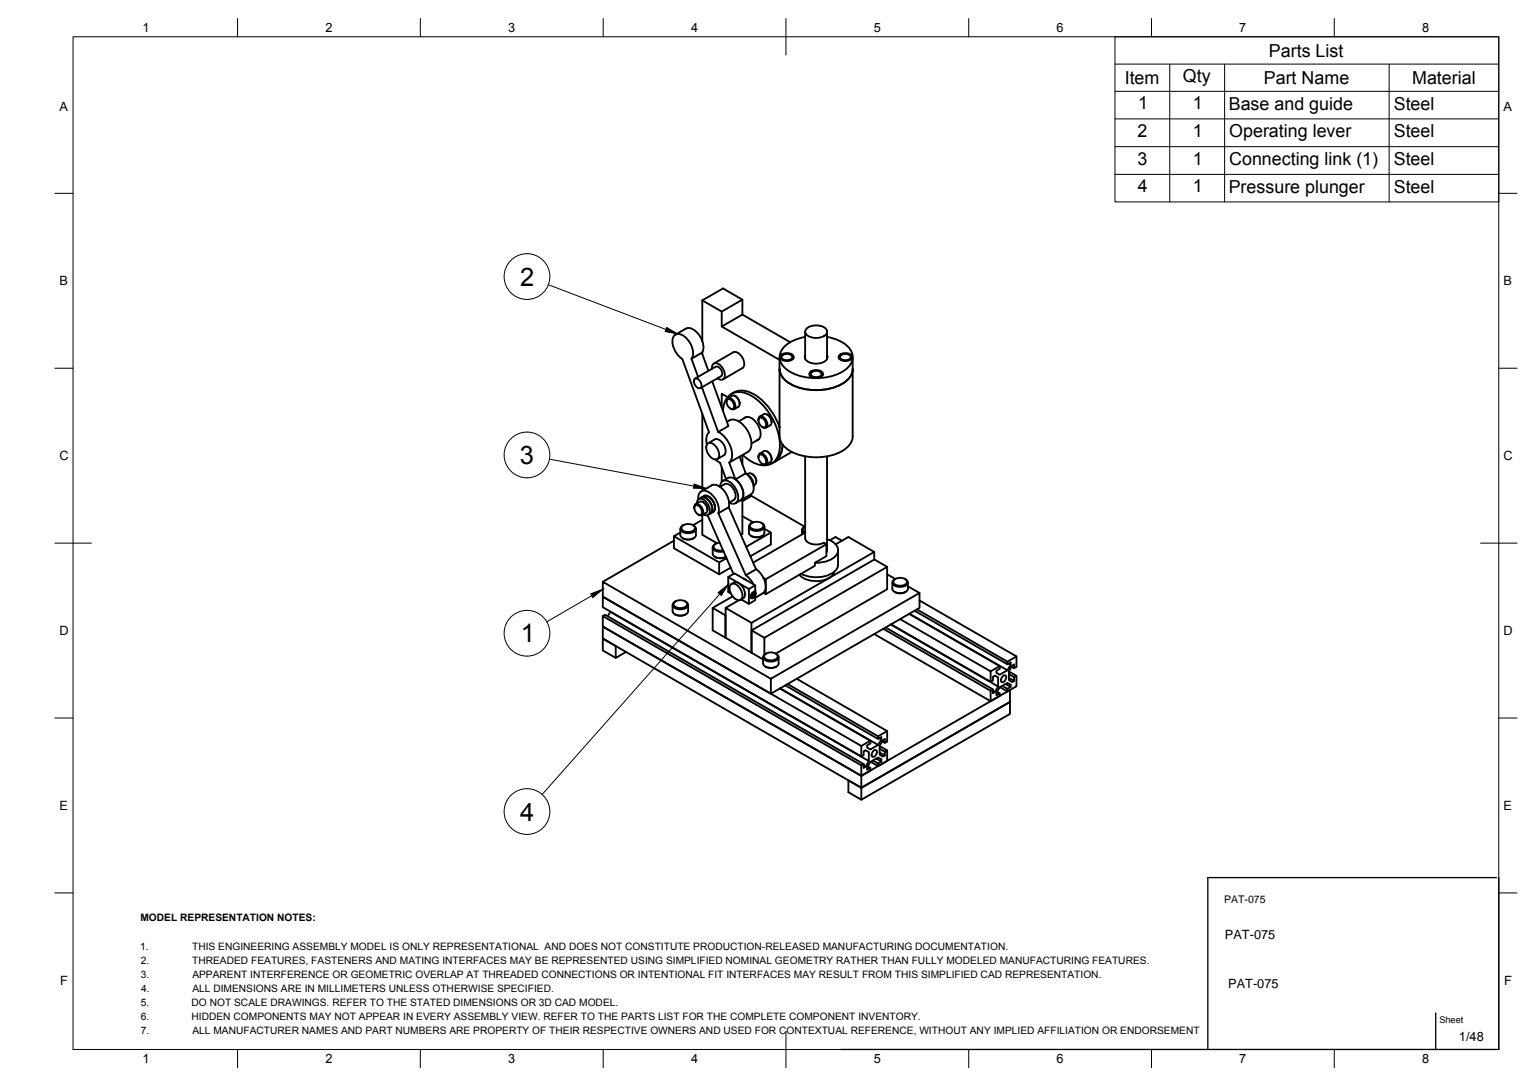
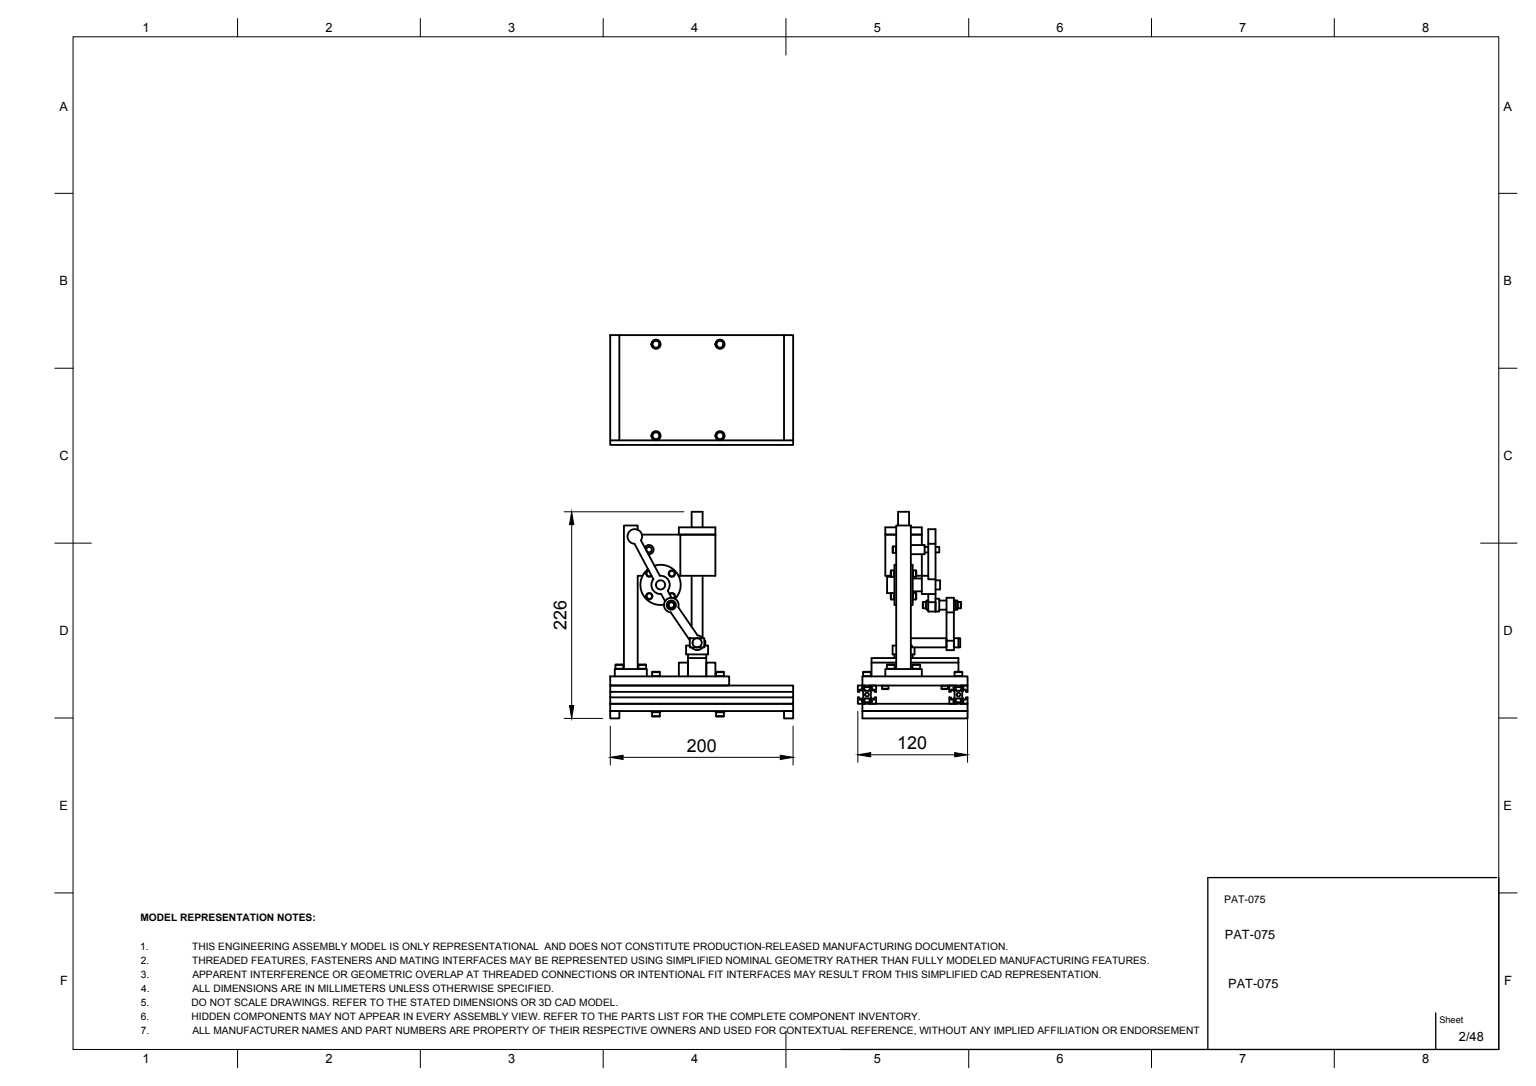
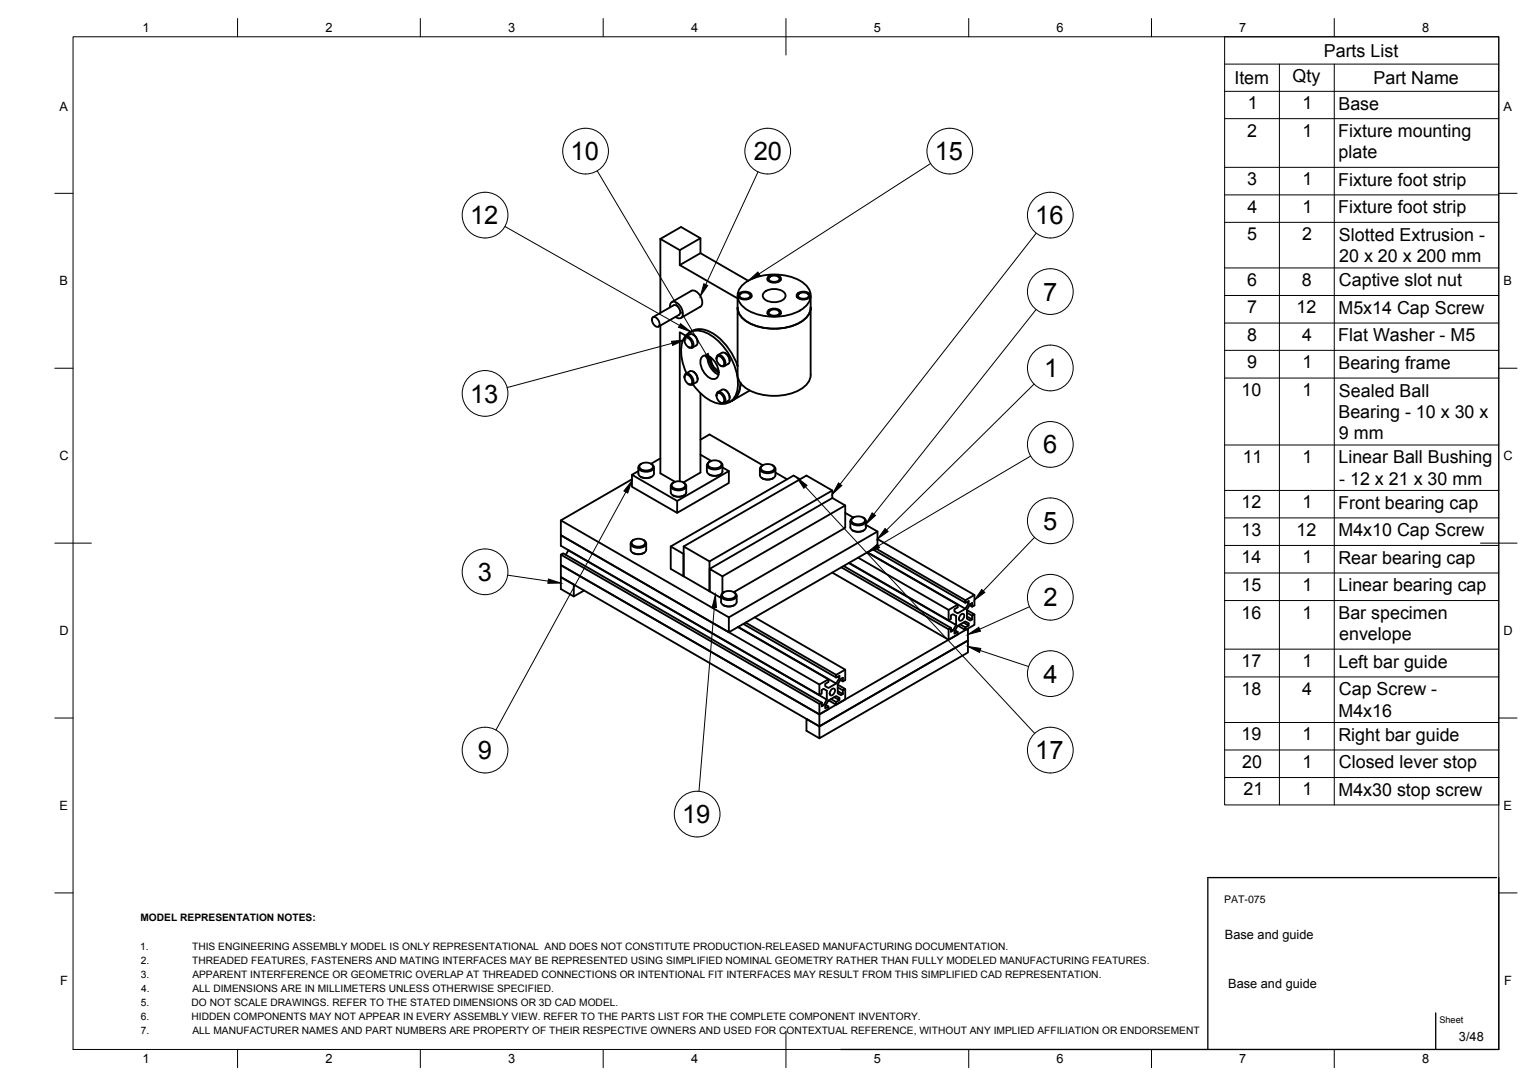
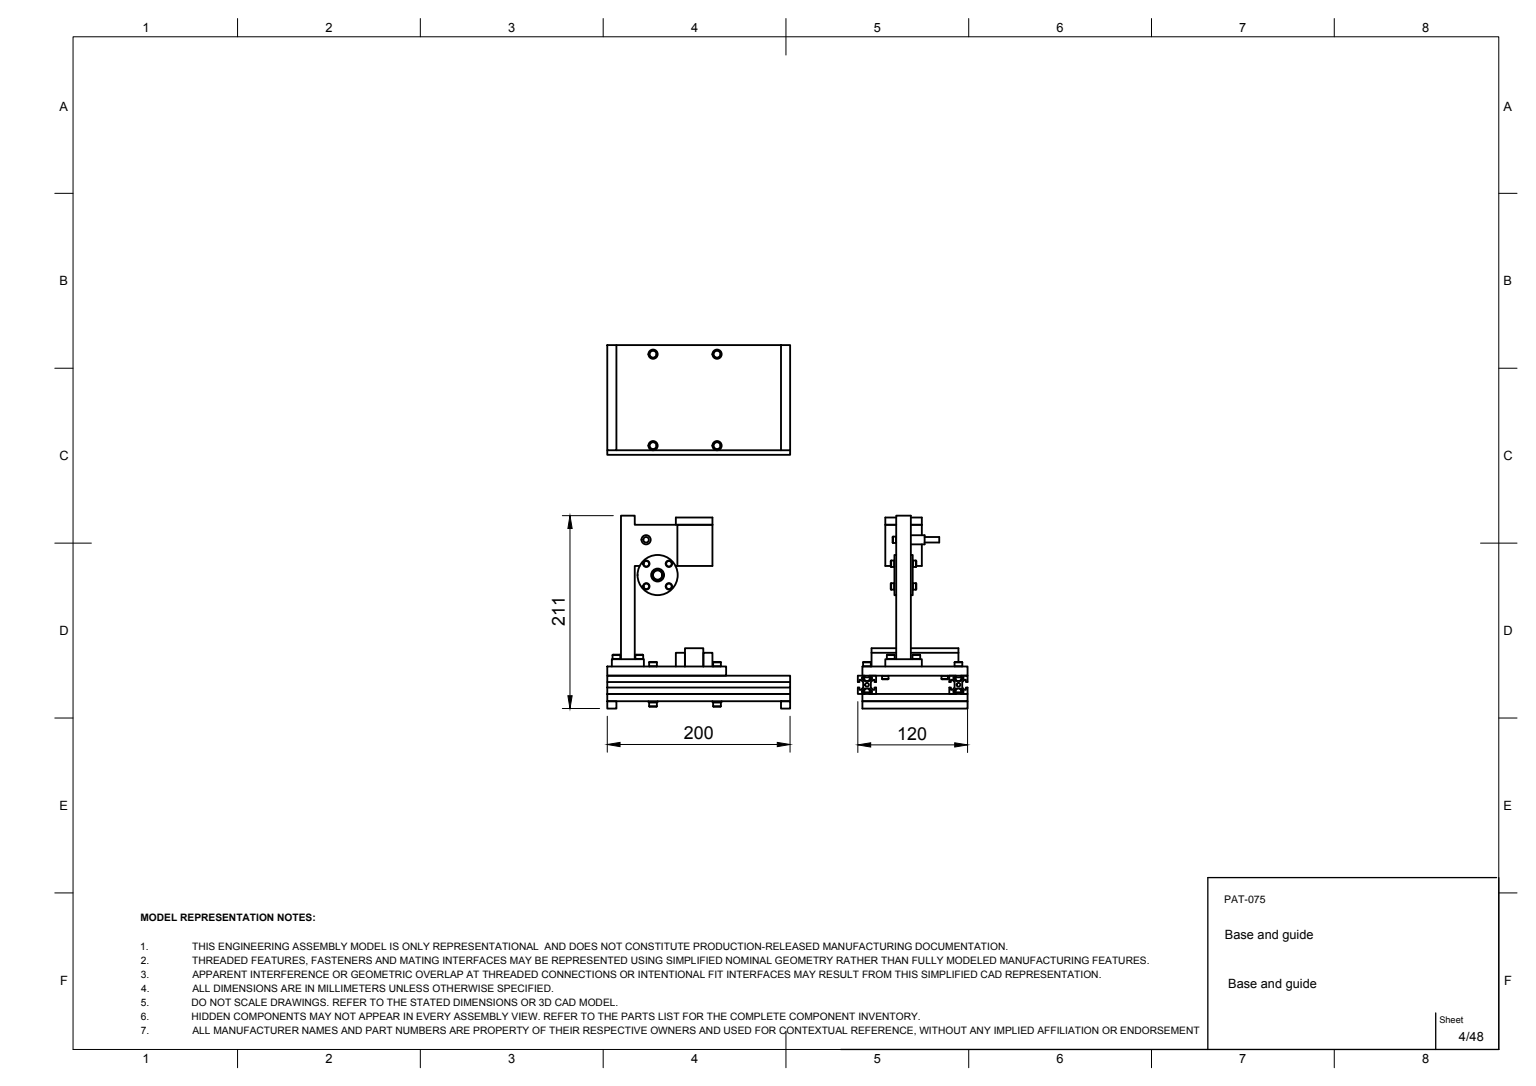
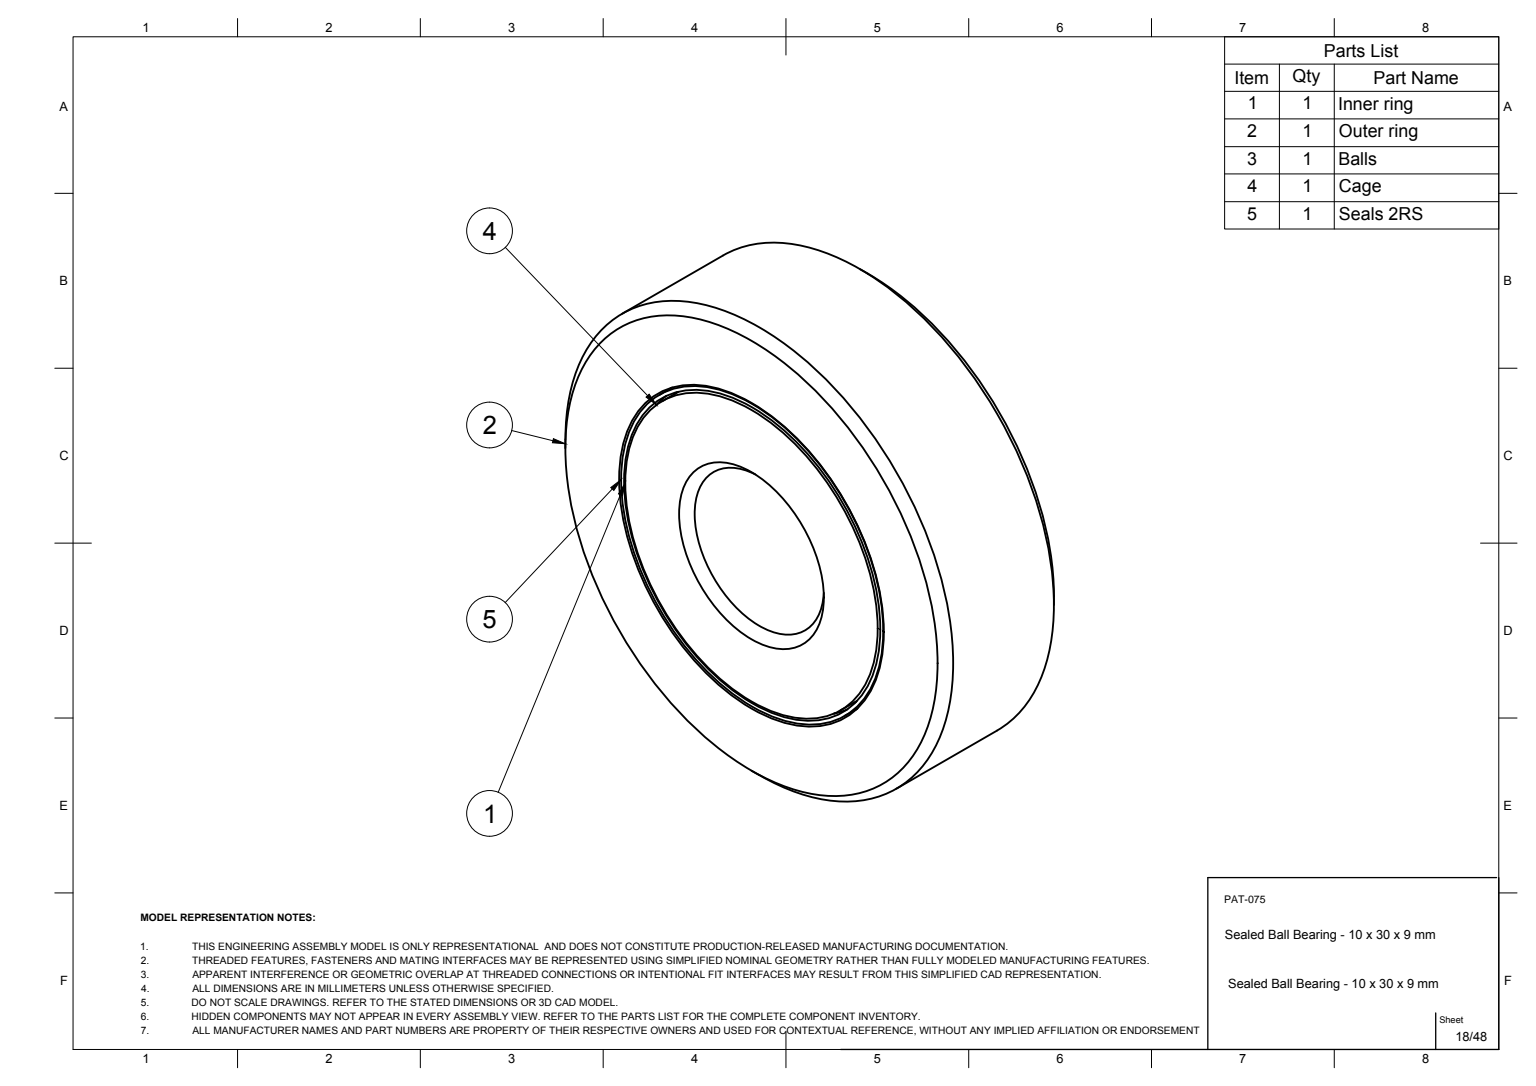
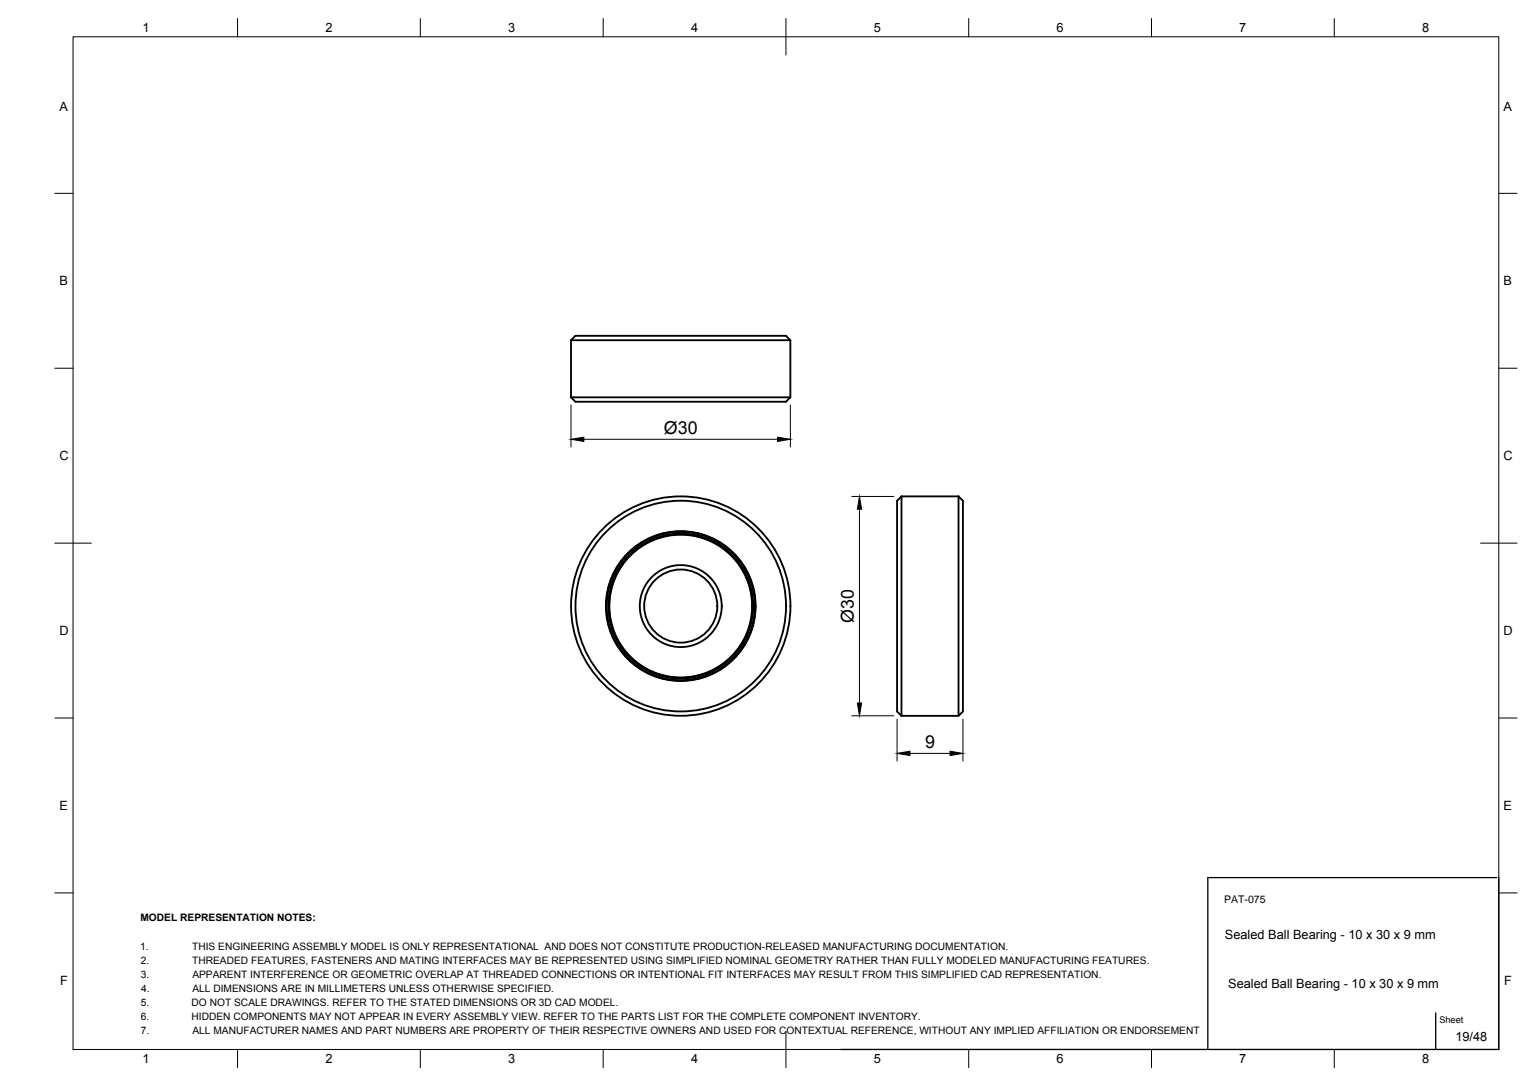
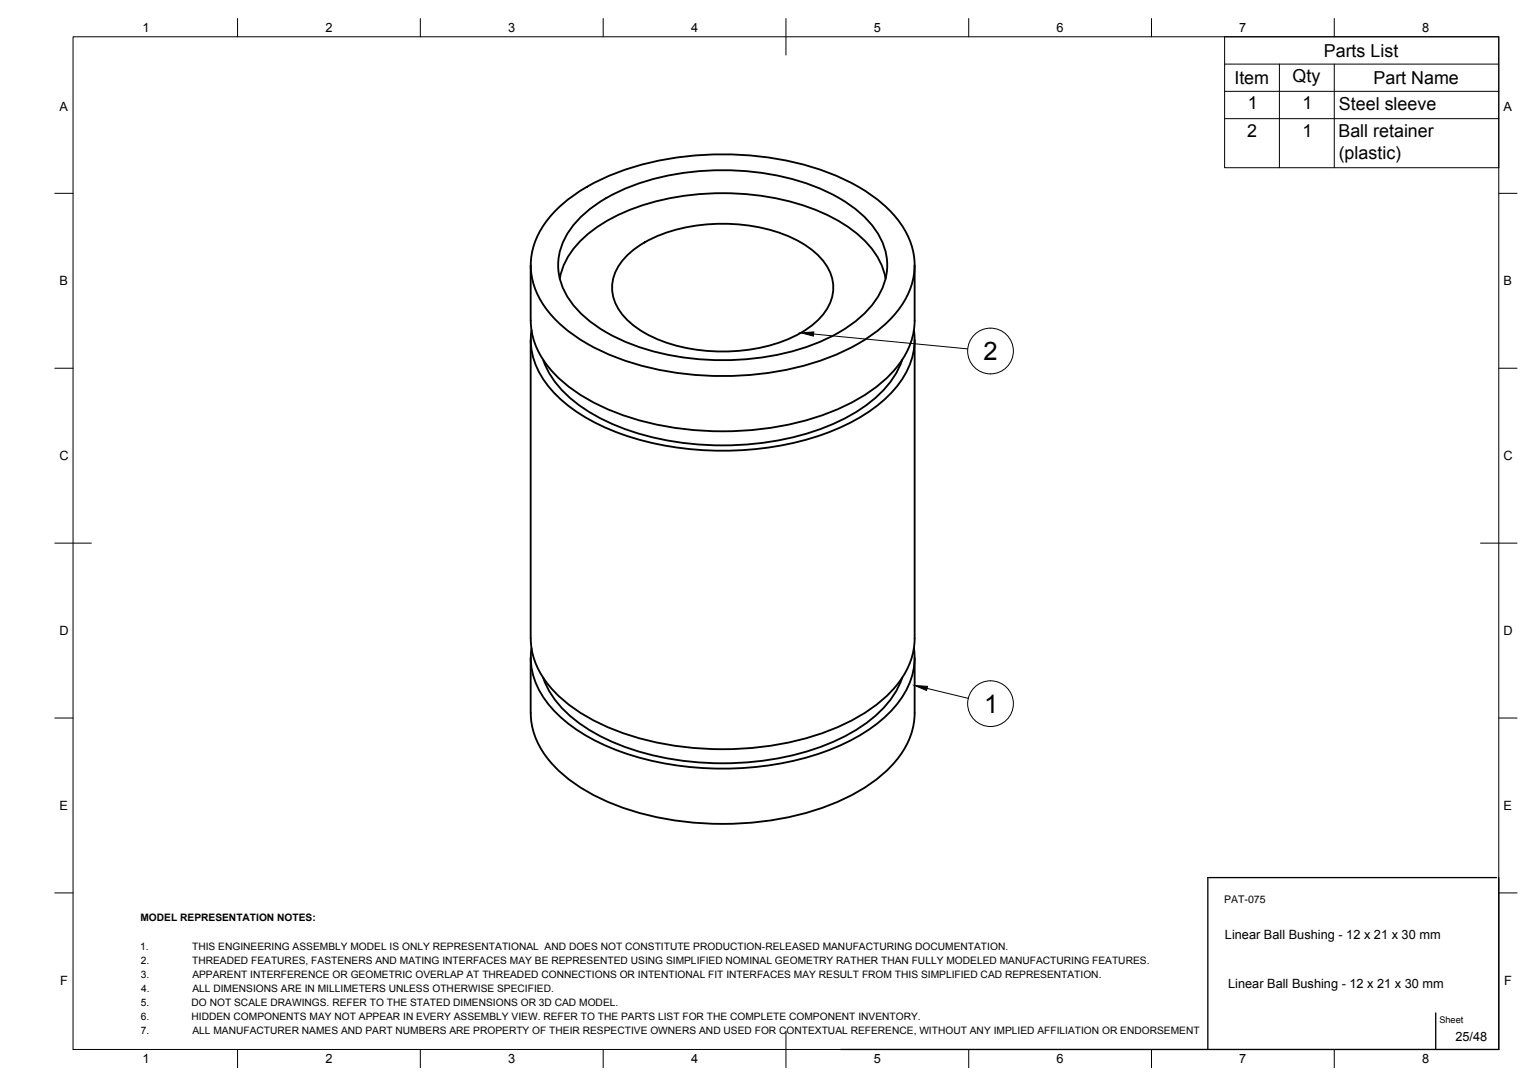
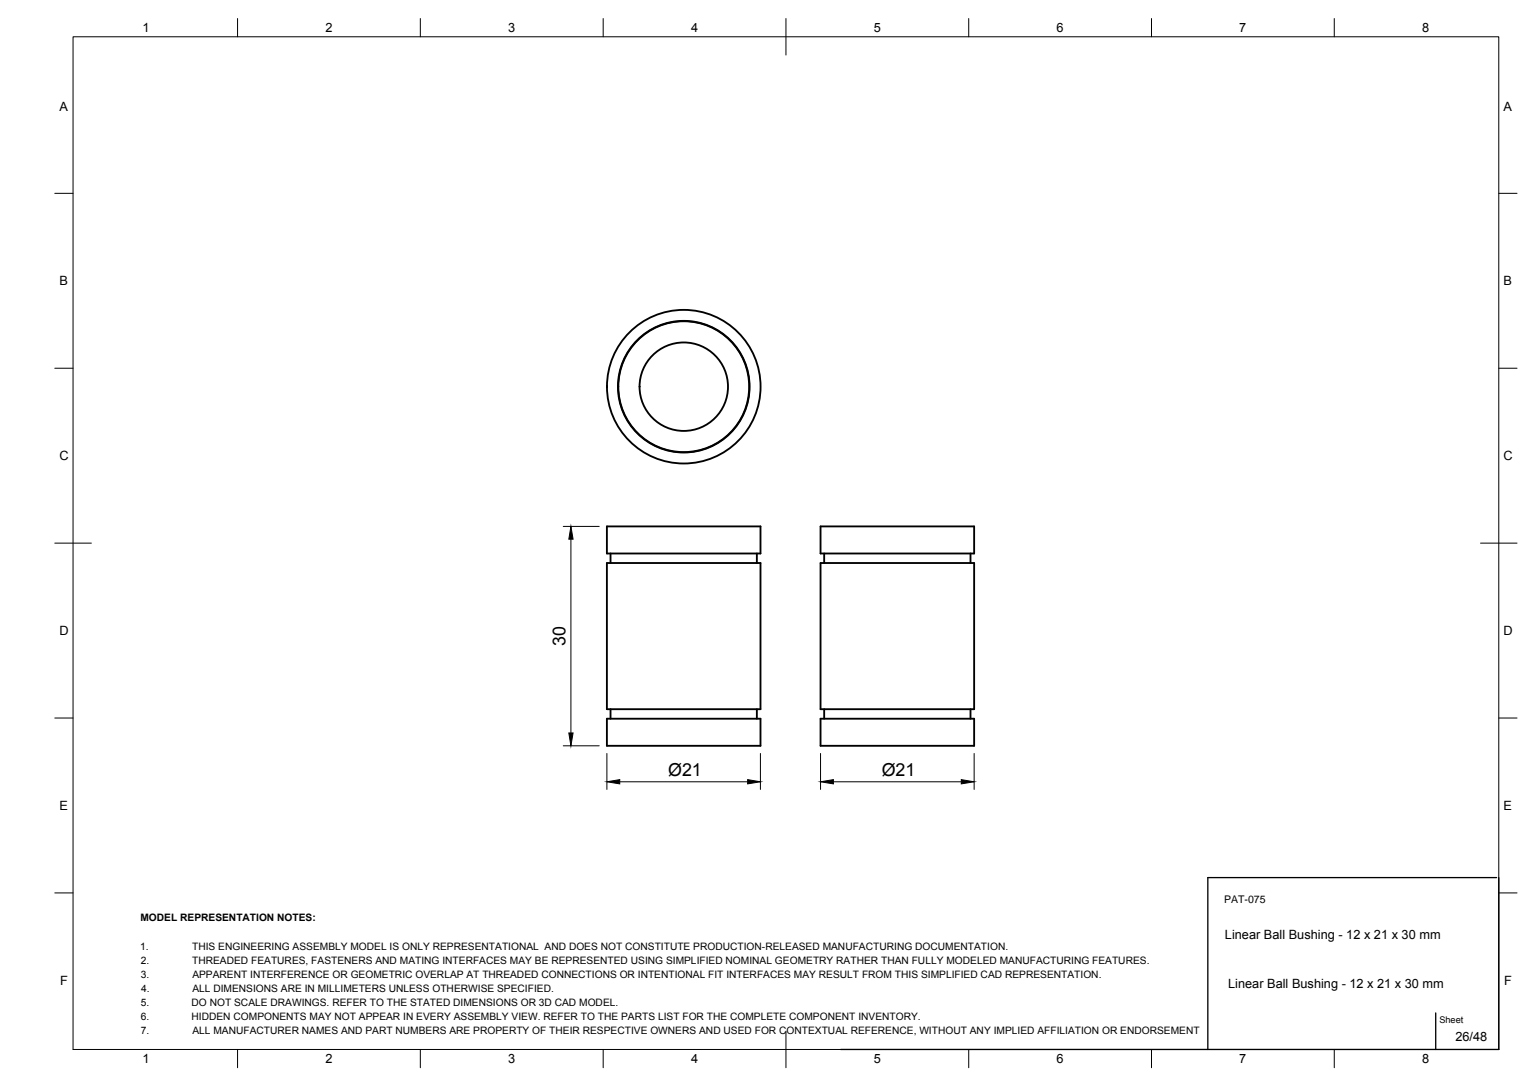
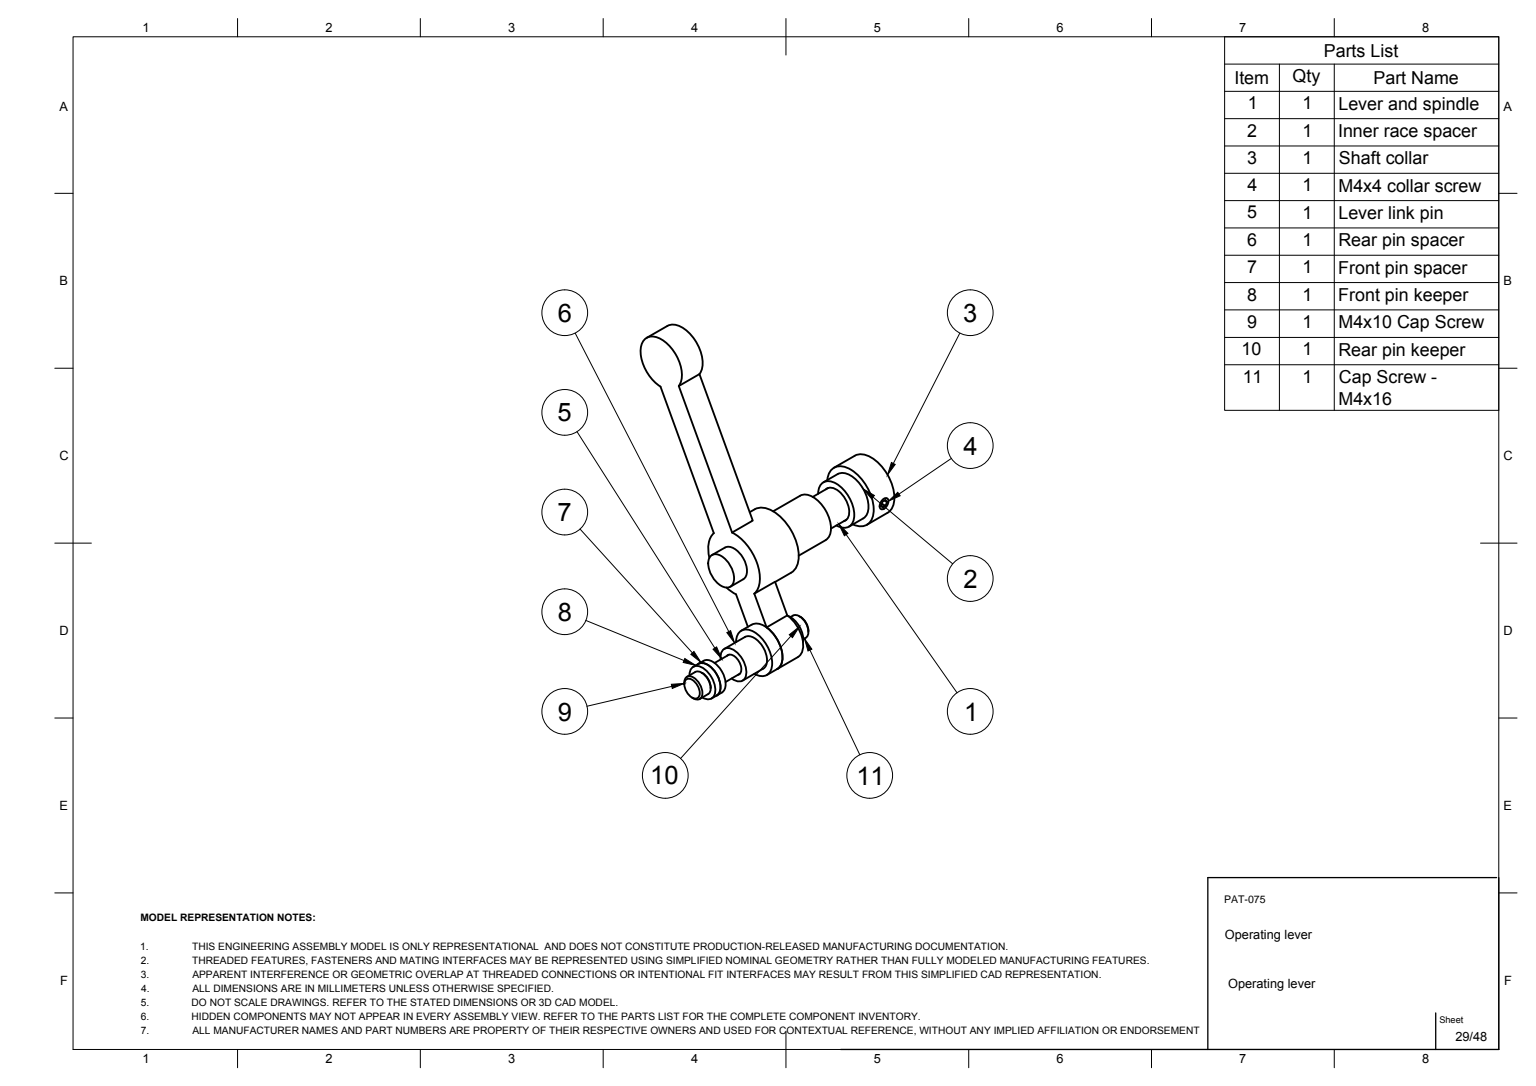
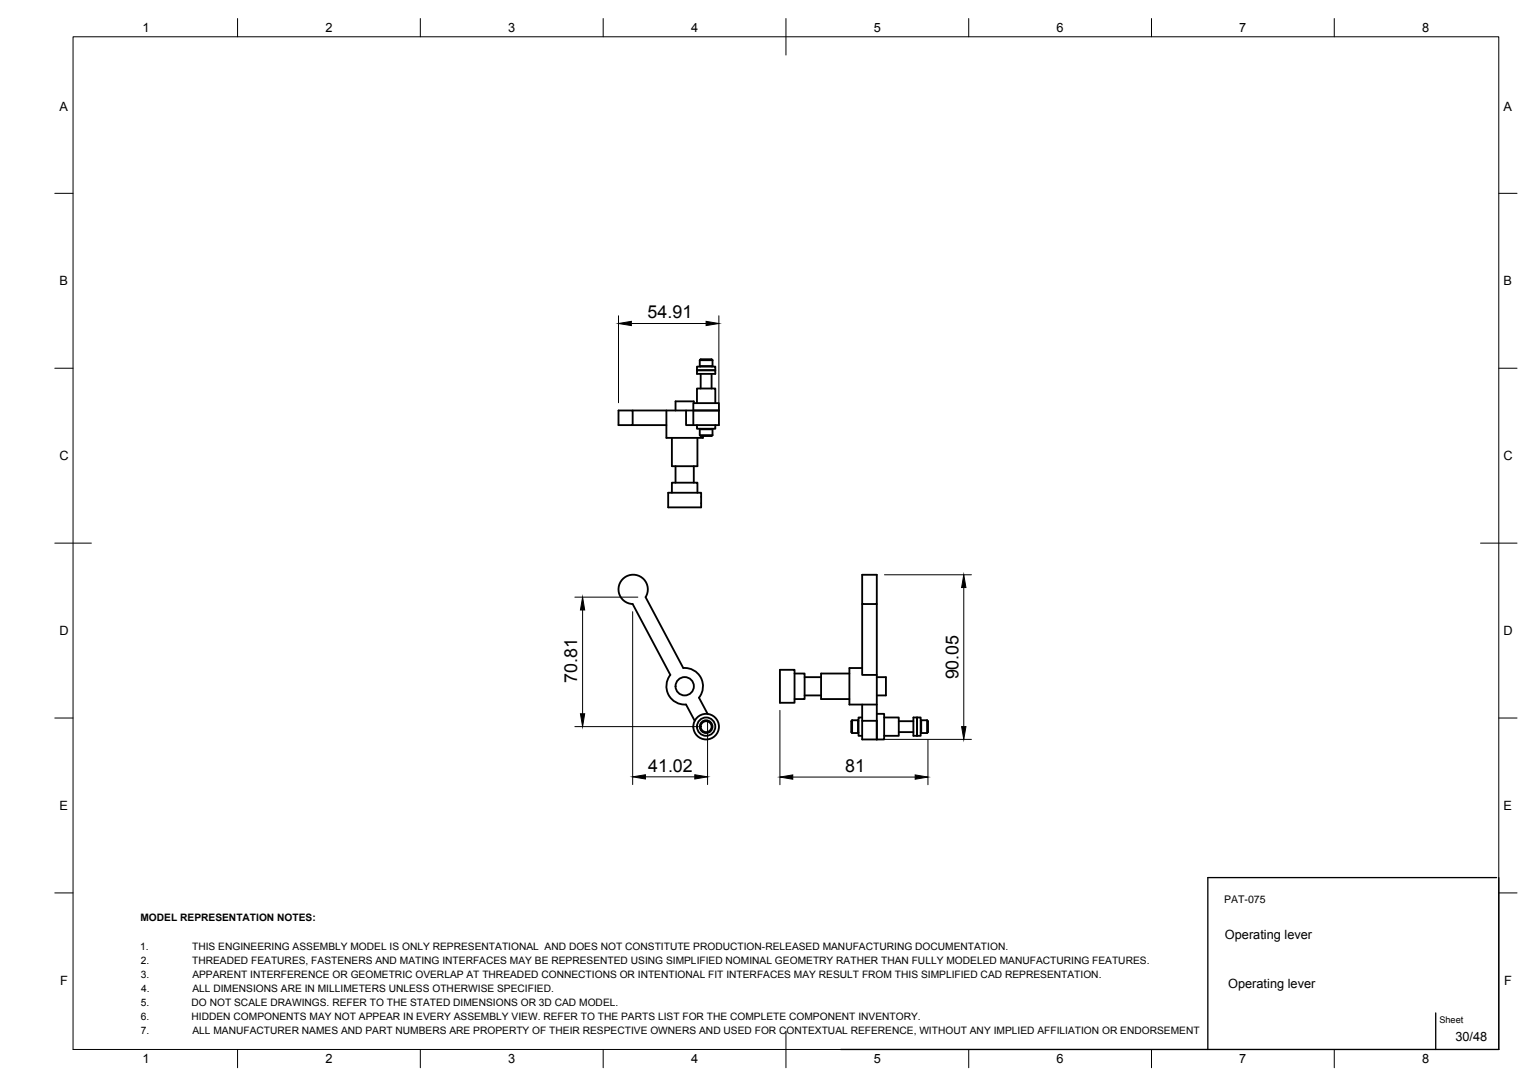
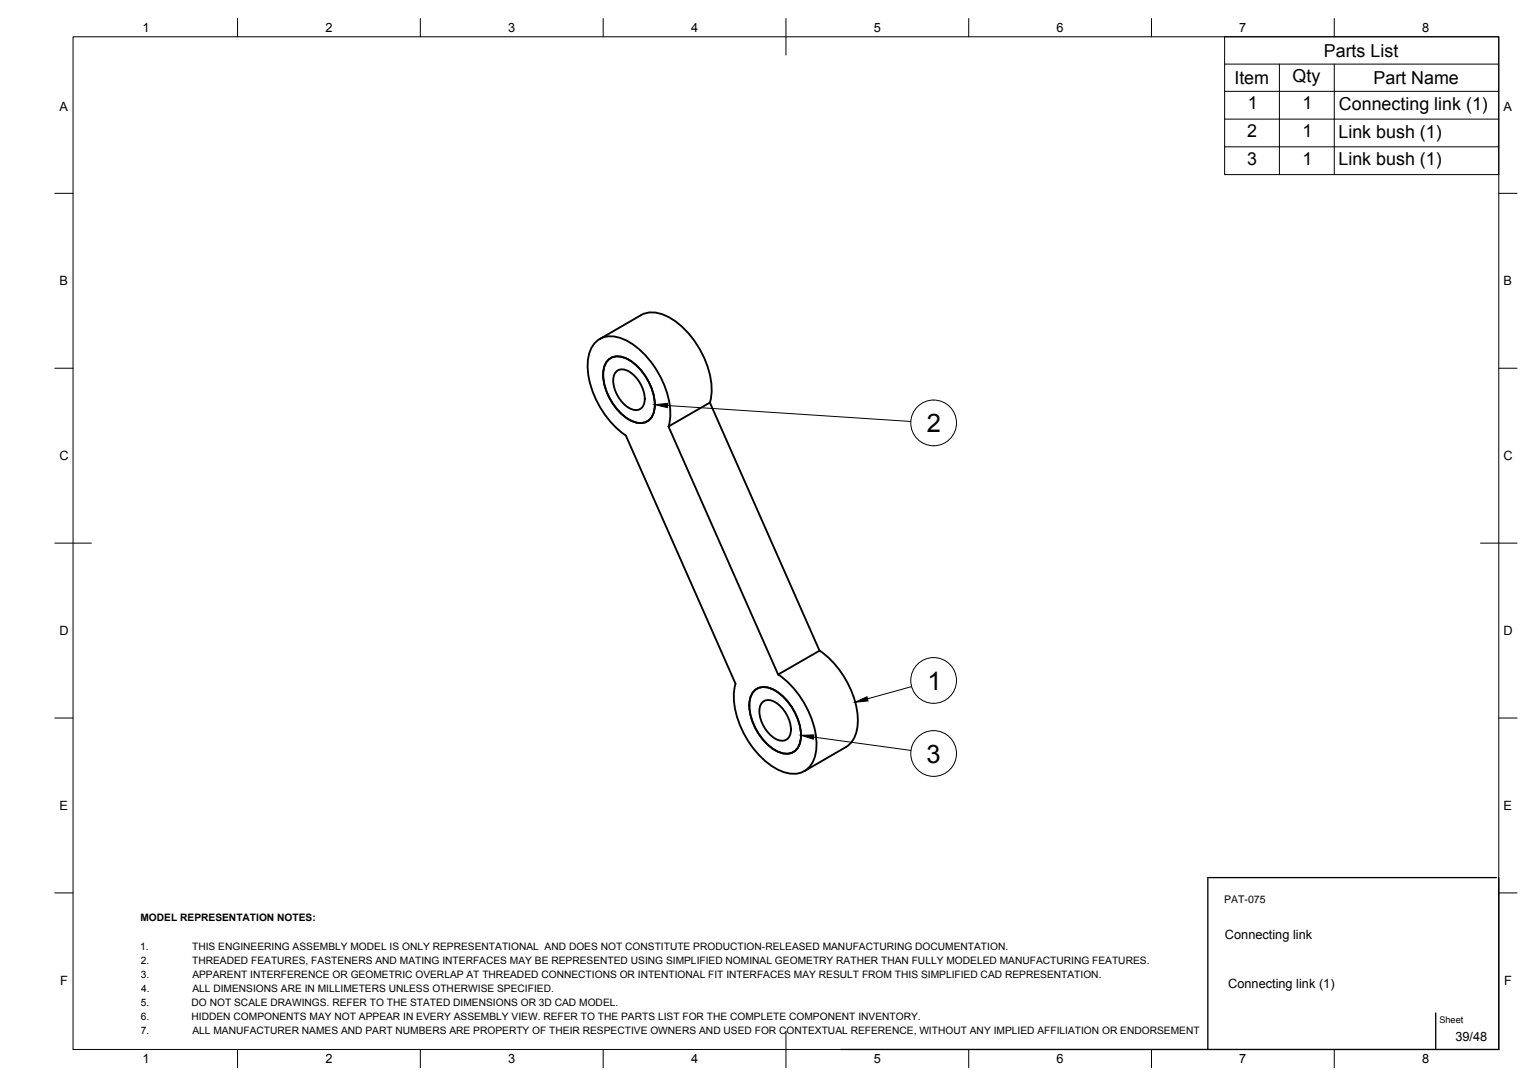
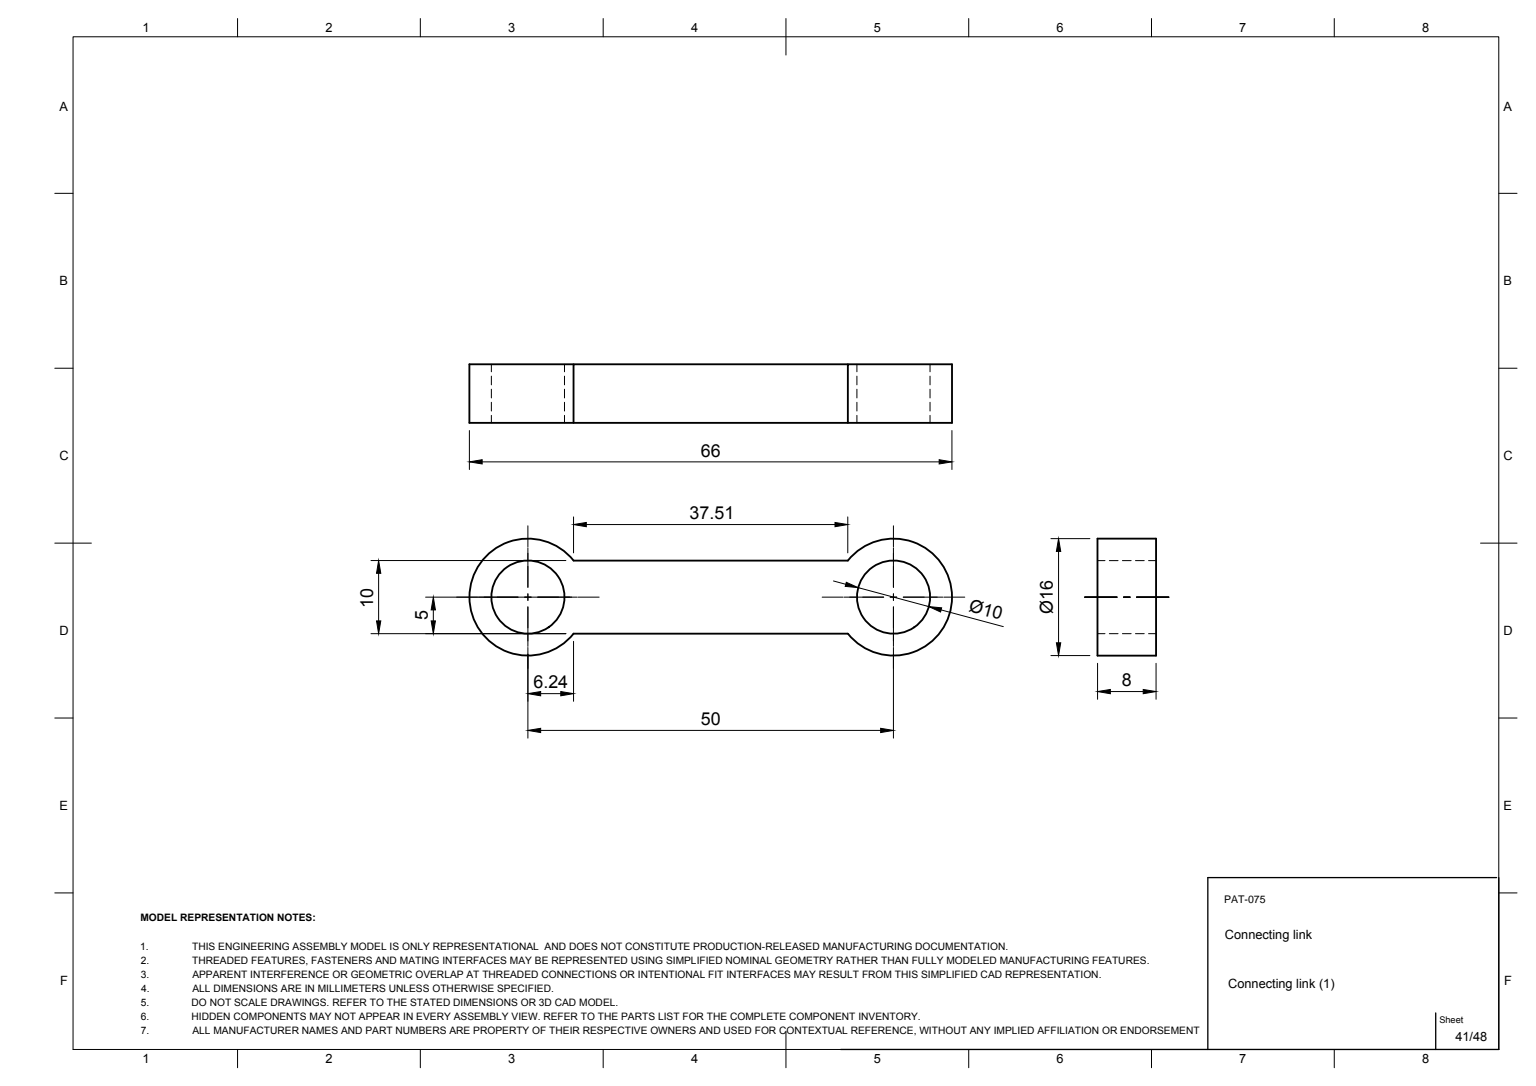
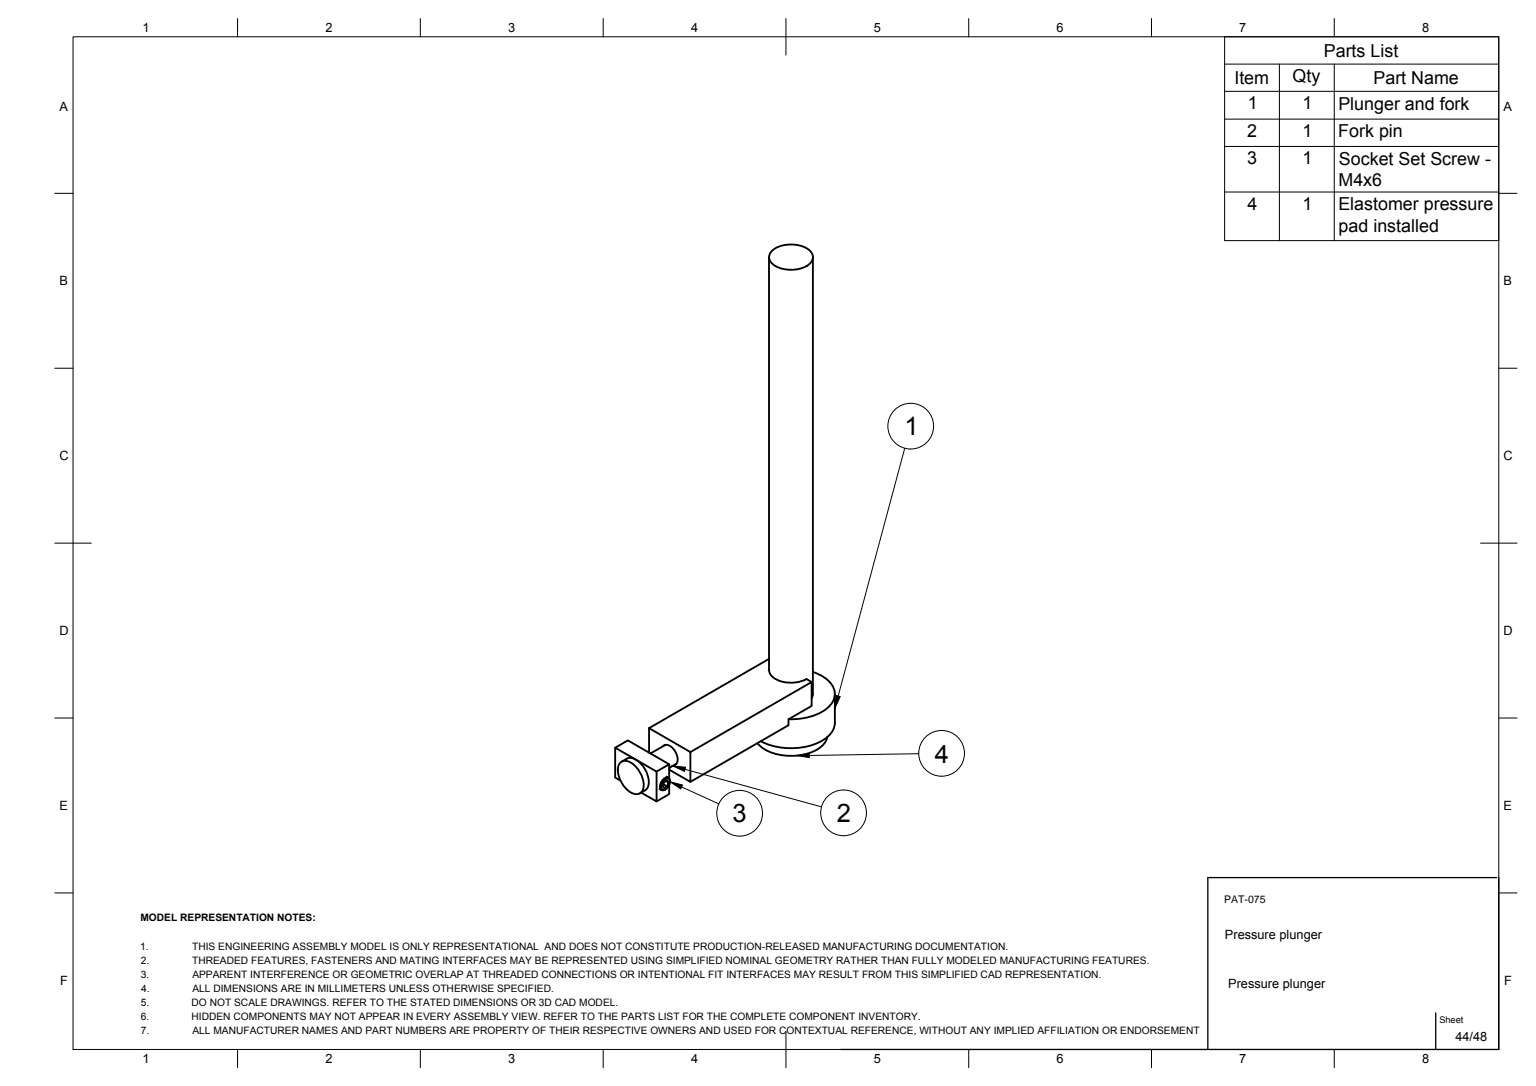
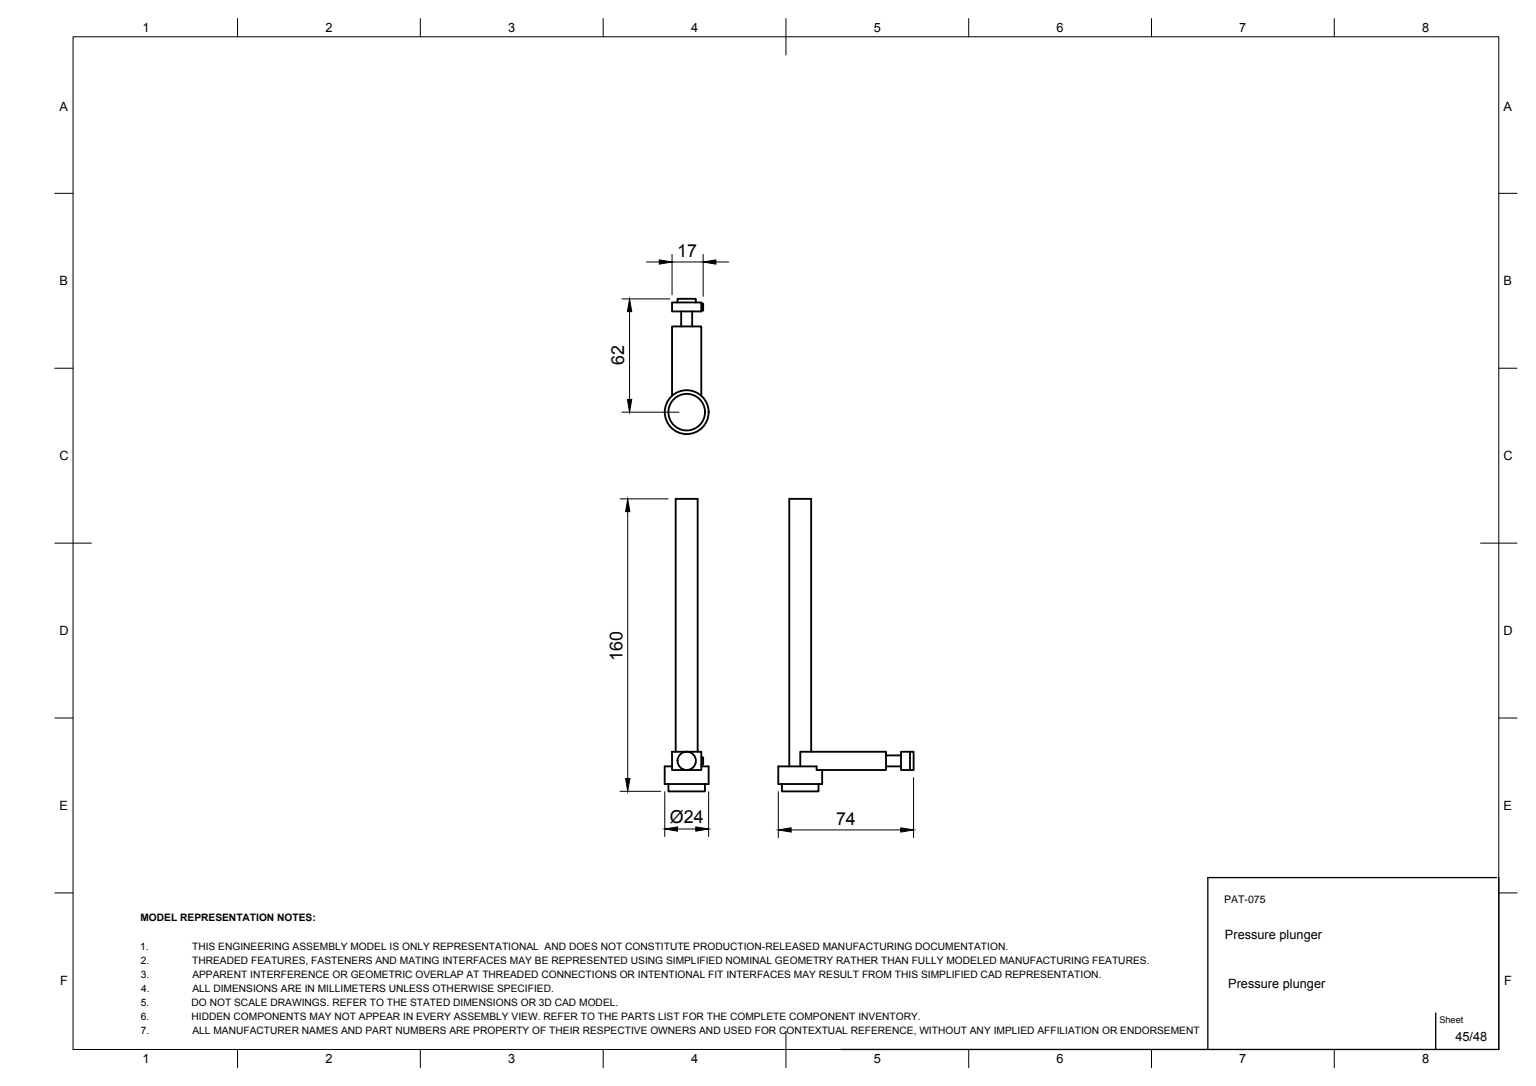
ISO-10303-21;
HEADER;
/* Generated by software containing ST-Developer
 * from STEP Tools, Inc. (www.steptools.com) 
 */

FILE_DESCRIPTION(
/* description */ ('Over-Centre Plunger Toggle Clamp on Slotted Fixture Frame'),
/* implementation_level */ '2;1');

FILE_NAME(
/* name */ 
'PAT-075',
/* time_stamp */ '2026-10-28T03:23:24-07:00',
/* author */ (''),
/* organization */ (''),
/* preprocessor_version */ 'ST-DEVELOPER v20.2',
/* originating_system */ 'Autodesk Translation Framework v15.17.0.0',
/* authorisation */ '');

FILE_SCHEMA (('AUTOMOTIVE_DESIGN { 1 0 10303 214 3 1 1 }'));
ENDSEC;

DATA;
#10=MECHANICAL_DESIGN_GEOMETRIC_PRESENTATION_REPRESENTATION('',(#513,#514,
#515,#516,#517,#518,#519,#520,#521,#522,#523,#524,#525,#526,#527,#528,#529,
#530,#531,#532,#533,#534,#535,#536,#537,#538,#539,#540,#541,#542,#543,#544,
#545,#546,#547,#548,#549,#550,#551,#552,#553,#554,#555,#556,#557,#558,#559,
#560,#561,#562,#563),#15212);
#11=ITEM_DEFINED_TRANSFORMATION($,$,#9165,#9293);
#12=ITEM_DEFINED_TRANSFORMATION($,$,#9185,#9294);
#13=ITEM_DEFINED_TRANSFORMATION($,$,#9205,#9295);
#14=ITEM_DEFINED_TRANSFORMATION($,$,#9222,#9296);
#15=ITEM_DEFINED_TRANSFORMATION($,$,#9276,#9297);
#16=ITEM_DEFINED_TRANSFORMATION($,$,#9299,#9348);
#17=ITEM_DEFINED_TRANSFORMATION($,$,#9331,#9349);
#18=ITEM_DEFINED_TRANSFORMATION($,$,#8765,#9565);
#19=ITEM_DEFINED_TRANSFORMATION($,$,#8808,#9566);
#20=ITEM_DEFINED_TRANSFORMATION($,$,#8827,#9567);
#21=ITEM_DEFINED_TRANSFORMATION($,$,#8834,#9568);
#22=ITEM_DEFINED_TRANSFORMATION($,$,#8841,#9569);
#23=ITEM_DEFINED_TRANSFORMATION($,$,#8916,#9570);
#24=ITEM_DEFINED_TRANSFORMATION($,$,#8941,#9571);
#25=ITEM_DEFINED_TRANSFORMATION($,$,#8966,#9572);
#26=ITEM_DEFINED_TRANSFORMATION($,$,#9007,#9573);
#27=ITEM_DEFINED_TRANSFORMATION($,$,#9014,#9574);
#28=ITEM_DEFINED_TRANSFORMATION($,$,#9029,#9575);
#29=ITEM_DEFINED_TRANSFORMATION($,$,#9044,#9576);
#30=ITEM_DEFINED_TRANSFORMATION($,$,#9058,#9577);
#31=ITEM_DEFINED_TRANSFORMATION($,$,#9108,#9578);
#32=ITEM_DEFINED_TRANSFORMATION($,$,#9140,#9579);
#33=ITEM_DEFINED_TRANSFORMATION($,$,#9108,#9580);
#34=ITEM_DEFINED_TRANSFORMATION($,$,#9129,#9581);
#35=ITEM_DEFINED_TRANSFORMATION($,$,#9140,#9582);
#36=ITEM_DEFINED_TRANSFORMATION($,$,#9108,#9583);
#37=ITEM_DEFINED_TRANSFORMATION($,$,#9140,#9584);
#38=ITEM_DEFINED_TRANSFORMATION($,$,#9108,#9585);
#39=ITEM_DEFINED_TRANSFORMATION($,$,#9129,#9586);
#40=ITEM_DEFINED_TRANSFORMATION($,$,#9140,#9587);
#41=ITEM_DEFINED_TRANSFORMATION($,$,#9058,#9588);
#42=ITEM_DEFINED_TRANSFORMATION($,$,#9108,#9589);
#43=ITEM_DEFINED_TRANSFORMATION($,$,#9140,#9590);
#44=ITEM_DEFINED_TRANSFORMATION($,$,#9108,#9591);
#45=ITEM_DEFINED_TRANSFORMATION($,$,#9129,#9592);
#46=ITEM_DEFINED_TRANSFORMATION($,$,#9140,#9593);
#47=ITEM_DEFINED_TRANSFORMATION($,$,#9108,#9594);
#48=ITEM_DEFINED_TRANSFORMATION($,$,#9140,#9595);
#49=ITEM_DEFINED_TRANSFORMATION($,$,#9108,#9596);
#50=ITEM_DEFINED_TRANSFORMATION($,$,#9129,#9597);
#51=ITEM_DEFINED_TRANSFORMATION($,$,#9140,#9598);
#52=ITEM_DEFINED_TRANSFORMATION($,$,#9140,#9599);
#53=ITEM_DEFINED_TRANSFORMATION($,$,#9140,#9600);
#54=ITEM_DEFINED_TRANSFORMATION($,$,#9140,#9601);
#55=ITEM_DEFINED_TRANSFORMATION($,$,#9140,#9602);
#56=ITEM_DEFINED_TRANSFORMATION($,$,#9164,#9603);
#57=ITEM_DEFINED_TRANSFORMATION($,$,#9298,#9604);
#58=ITEM_DEFINED_TRANSFORMATION($,$,#9515,#9605);
#59=ITEM_DEFINED_TRANSFORMATION($,$,#9515,#9606);
#60=ITEM_DEFINED_TRANSFORMATION($,$,#9515,#9607);
#61=ITEM_DEFINED_TRANSFORMATION($,$,#9515,#9608);
#62=ITEM_DEFINED_TRANSFORMATION($,$,#9515,#9609);
#63=ITEM_DEFINED_TRANSFORMATION($,$,#9515,#9610);
#64=ITEM_DEFINED_TRANSFORMATION($,$,#9515,#9611);
#65=ITEM_DEFINED_TRANSFORMATION($,$,#9515,#9612);
#66=ITEM_DEFINED_TRANSFORMATION($,$,#9515,#9613);
#67=ITEM_DEFINED_TRANSFORMATION($,$,#9515,#9614);
#68=ITEM_DEFINED_TRANSFORMATION($,$,#9515,#9615);
#69=ITEM_DEFINED_TRANSFORMATION($,$,#9515,#9616);
#70=ITEM_DEFINED_TRANSFORMATION($,$,#9539,#9617);
#71=ITEM_DEFINED_TRANSFORMATION($,$,#9539,#9618);
#72=ITEM_DEFINED_TRANSFORMATION($,$,#9539,#9619);
#73=ITEM_DEFINED_TRANSFORMATION($,$,#9539,#9620);
#74=ITEM_DEFINED_TRANSFORMATION($,$,#9350,#9621);
#75=ITEM_DEFINED_TRANSFORMATION($,$,#9381,#9622);
#76=ITEM_DEFINED_TRANSFORMATION($,$,#9418,#9623);
#77=ITEM_DEFINED_TRANSFORMATION($,$,#9427,#9624);
#78=ITEM_DEFINED_TRANSFORMATION($,$,#9442,#9625);
#79=ITEM_DEFINED_TRANSFORMATION($,$,#9464,#9626);
#80=ITEM_DEFINED_TRANSFORMATION($,$,#9473,#9627);
#81=ITEM_DEFINED_TRANSFORMATION($,$,#9482,#9628);
#82=ITEM_DEFINED_TRANSFORMATION($,$,#9491,#9629);
#83=ITEM_DEFINED_TRANSFORMATION($,$,#9500,#9630);
#84=ITEM_DEFINED_TRANSFORMATION($,$,#9515,#9631);
#85=ITEM_DEFINED_TRANSFORMATION($,$,#9539,#9632);
#86=ITEM_DEFINED_TRANSFORMATION($,$,#9634,#9669);
#87=ITEM_DEFINED_TRANSFORMATION($,$,#9651,#9670);
#88=ITEM_DEFINED_TRANSFORMATION($,$,#9660,#9671);
#89=ITEM_DEFINED_TRANSFORMATION($,$,#9673,#9746);
#90=ITEM_DEFINED_TRANSFORMATION($,$,#9713,#9747);
#91=ITEM_DEFINED_TRANSFORMATION($,$,#9723,#9748);
#92=ITEM_DEFINED_TRANSFORMATION($,$,#9729,#9749);
#93=ITEM_DEFINED_TRANSFORMATION($,$,#8764,#9750);
#94=ITEM_DEFINED_TRANSFORMATION($,$,#9380,#9751);
#95=ITEM_DEFINED_TRANSFORMATION($,$,#9633,#9752);
#96=ITEM_DEFINED_TRANSFORMATION($,$,#9672,#9753);
#97=(
REPRESENTATION_RELATIONSHIP($,$,#15420,#15419)
REPRESENTATION_RELATIONSHIP_WITH_TRANSFORMATION(#11)
SHAPE_REPRESENTATION_RELATIONSHIP()
);
#98=(
REPRESENTATION_RELATIONSHIP($,$,#15421,#15419)
REPRESENTATION_RELATIONSHIP_WITH_TRANSFORMATION(#12)
SHAPE_REPRESENTATION_RELATIONSHIP()
);
#99=(
REPRESENTATION_RELATIONSHIP($,$,#15422,#15419)
REPRESENTATION_RELATIONSHIP_WITH_TRANSFORMATION(#13)
SHAPE_REPRESENTATION_RELATIONSHIP()
);
#100=(
REPRESENTATION_RELATIONSHIP($,$,#15423,#15419)
REPRESENTATION_RELATIONSHIP_WITH_TRANSFORMATION(#14)
SHAPE_REPRESENTATION_RELATIONSHIP()
);
#101=(
REPRESENTATION_RELATIONSHIP($,$,#15424,#15419)
REPRESENTATION_RELATIONSHIP_WITH_TRANSFORMATION(#15)
SHAPE_REPRESENTATION_RELATIONSHIP()
);
#102=(
REPRESENTATION_RELATIONSHIP($,$,#15426,#15425)
REPRESENTATION_RELATIONSHIP_WITH_TRANSFORMATION(#16)
SHAPE_REPRESENTATION_RELATIONSHIP()
);
#103=(
REPRESENTATION_RELATIONSHIP($,$,#15427,#15425)
REPRESENTATION_RELATIONSHIP_WITH_TRANSFORMATION(#17)
SHAPE_REPRESENTATION_RELATIONSHIP()
);
#104=(
REPRESENTATION_RELATIONSHIP($,$,#15403,#15402)
REPRESENTATION_RELATIONSHIP_WITH_TRANSFORMATION(#18)
SHAPE_REPRESENTATION_RELATIONSHIP()
);
#105=(
REPRESENTATION_RELATIONSHIP($,$,#15404,#15402)
REPRESENTATION_RELATIONSHIP_WITH_TRANSFORMATION(#19)
SHAPE_REPRESENTATION_RELATIONSHIP()
);
#106=(
REPRESENTATION_RELATIONSHIP($,$,#15405,#15402)
REPRESENTATION_RELATIONSHIP_WITH_TRANSFORMATION(#20)
SHAPE_REPRESENTATION_RELATIONSHIP()
);
#107=(
REPRESENTATION_RELATIONSHIP($,$,#15406,#15402)
REPRESENTATION_RELATIONSHIP_WITH_TRANSFORMATION(#21)
SHAPE_REPRESENTATION_RELATIONSHIP()
);
#108=(
REPRESENTATION_RELATIONSHIP($,$,#15407,#15402)
REPRESENTATION_RELATIONSHIP_WITH_TRANSFORMATION(#22)
SHAPE_REPRESENTATION_RELATIONSHIP()
);
#109=(
REPRESENTATION_RELATIONSHIP($,$,#15408,#15402)
REPRESENTATION_RELATIONSHIP_WITH_TRANSFORMATION(#23)
SHAPE_REPRESENTATION_RELATIONSHIP()
);
#110=(
REPRESENTATION_RELATIONSHIP($,$,#15409,#15402)
REPRESENTATION_RELATIONSHIP_WITH_TRANSFORMATION(#24)
SHAPE_REPRESENTATION_RELATIONSHIP()
);
#111=(
REPRESENTATION_RELATIONSHIP($,$,#15410,#15402)
REPRESENTATION_RELATIONSHIP_WITH_TRANSFORMATION(#25)
SHAPE_REPRESENTATION_RELATIONSHIP()
);
#112=(
REPRESENTATION_RELATIONSHIP($,$,#15411,#15402)
REPRESENTATION_RELATIONSHIP_WITH_TRANSFORMATION(#26)
SHAPE_REPRESENTATION_RELATIONSHIP()
);
#113=(
REPRESENTATION_RELATIONSHIP($,$,#15412,#15402)
REPRESENTATION_RELATIONSHIP_WITH_TRANSFORMATION(#27)
SHAPE_REPRESENTATION_RELATIONSHIP()
);
#114=(
REPRESENTATION_RELATIONSHIP($,$,#15413,#15402)
REPRESENTATION_RELATIONSHIP_WITH_TRANSFORMATION(#28)
SHAPE_REPRESENTATION_RELATIONSHIP()
);
#115=(
REPRESENTATION_RELATIONSHIP($,$,#15414,#15402)
REPRESENTATION_RELATIONSHIP_WITH_TRANSFORMATION(#29)
SHAPE_REPRESENTATION_RELATIONSHIP()
);
#116=(
REPRESENTATION_RELATIONSHIP($,$,#15415,#15402)
REPRESENTATION_RELATIONSHIP_WITH_TRANSFORMATION(#30)
SHAPE_REPRESENTATION_RELATIONSHIP()
);
#117=(
REPRESENTATION_RELATIONSHIP($,$,#15416,#15402)
REPRESENTATION_RELATIONSHIP_WITH_TRANSFORMATION(#31)
SHAPE_REPRESENTATION_RELATIONSHIP()
);
#118=(
REPRESENTATION_RELATIONSHIP($,$,#15418,#15402)
REPRESENTATION_RELATIONSHIP_WITH_TRANSFORMATION(#32)
SHAPE_REPRESENTATION_RELATIONSHIP()
);
#119=(
REPRESENTATION_RELATIONSHIP($,$,#15416,#15402)
REPRESENTATION_RELATIONSHIP_WITH_TRANSFORMATION(#33)
SHAPE_REPRESENTATION_RELATIONSHIP()
);
#120=(
REPRESENTATION_RELATIONSHIP($,$,#15417,#15402)
REPRESENTATION_RELATIONSHIP_WITH_TRANSFORMATION(#34)
SHAPE_REPRESENTATION_RELATIONSHIP()
);
#121=(
REPRESENTATION_RELATIONSHIP($,$,#15418,#15402)
REPRESENTATION_RELATIONSHIP_WITH_TRANSFORMATION(#35)
SHAPE_REPRESENTATION_RELATIONSHIP()
);
#122=(
REPRESENTATION_RELATIONSHIP($,$,#15416,#15402)
REPRESENTATION_RELATIONSHIP_WITH_TRANSFORMATION(#36)
SHAPE_REPRESENTATION_RELATIONSHIP()
);
#123=(
REPRESENTATION_RELATIONSHIP($,$,#15418,#15402)
REPRESENTATION_RELATIONSHIP_WITH_TRANSFORMATION(#37)
SHAPE_REPRESENTATION_RELATIONSHIP()
);
#124=(
REPRESENTATION_RELATIONSHIP($,$,#15416,#15402)
REPRESENTATION_RELATIONSHIP_WITH_TRANSFORMATION(#38)
SHAPE_REPRESENTATION_RELATIONSHIP()
);
#125=(
REPRESENTATION_RELATIONSHIP($,$,#15417,#15402)
REPRESENTATION_RELATIONSHIP_WITH_TRANSFORMATION(#39)
SHAPE_REPRESENTATION_RELATIONSHIP()
);
#126=(
REPRESENTATION_RELATIONSHIP($,$,#15418,#15402)
REPRESENTATION_RELATIONSHIP_WITH_TRANSFORMATION(#40)
SHAPE_REPRESENTATION_RELATIONSHIP()
);
#127=(
REPRESENTATION_RELATIONSHIP($,$,#15415,#15402)
REPRESENTATION_RELATIONSHIP_WITH_TRANSFORMATION(#41)
SHAPE_REPRESENTATION_RELATIONSHIP()
);
#128=(
REPRESENTATION_RELATIONSHIP($,$,#15416,#15402)
REPRESENTATION_RELATIONSHIP_WITH_TRANSFORMATION(#42)
SHAPE_REPRESENTATION_RELATIONSHIP()
);
#129=(
REPRESENTATION_RELATIONSHIP($,$,#15418,#15402)
REPRESENTATION_RELATIONSHIP_WITH_TRANSFORMATION(#43)
SHAPE_REPRESENTATION_RELATIONSHIP()
);
#130=(
REPRESENTATION_RELATIONSHIP($,$,#15416,#15402)
REPRESENTATION_RELATIONSHIP_WITH_TRANSFORMATION(#44)
SHAPE_REPRESENTATION_RELATIONSHIP()
);
#131=(
REPRESENTATION_RELATIONSHIP($,$,#15417,#15402)
REPRESENTATION_RELATIONSHIP_WITH_TRANSFORMATION(#45)
SHAPE_REPRESENTATION_RELATIONSHIP()
);
#132=(
REPRESENTATION_RELATIONSHIP($,$,#15418,#15402)
REPRESENTATION_RELATIONSHIP_WITH_TRANSFORMATION(#46)
SHAPE_REPRESENTATION_RELATIONSHIP()
);
#133=(
REPRESENTATION_RELATIONSHIP($,$,#15416,#15402)
REPRESENTATION_RELATIONSHIP_WITH_TRANSFORMATION(#47)
SHAPE_REPRESENTATION_RELATIONSHIP()
);
#134=(
REPRESENTATION_RELATIONSHIP($,$,#15418,#15402)
REPRESENTATION_RELATIONSHIP_WITH_TRANSFORMATION(#48)
SHAPE_REPRESENTATION_RELATIONSHIP()
);
#135=(
REPRESENTATION_RELATIONSHIP($,$,#15416,#15402)
REPRESENTATION_RELATIONSHIP_WITH_TRANSFORMATION(#49)
SHAPE_REPRESENTATION_RELATIONSHIP()
);
#136=(
REPRESENTATION_RELATIONSHIP($,$,#15417,#15402)
REPRESENTATION_RELATIONSHIP_WITH_TRANSFORMATION(#50)
SHAPE_REPRESENTATION_RELATIONSHIP()
);
#137=(
REPRESENTATION_RELATIONSHIP($,$,#15418,#15402)
REPRESENTATION_RELATIONSHIP_WITH_TRANSFORMATION(#51)
SHAPE_REPRESENTATION_RELATIONSHIP()
);
#138=(
REPRESENTATION_RELATIONSHIP($,$,#15418,#15402)
REPRESENTATION_RELATIONSHIP_WITH_TRANSFORMATION(#52)
SHAPE_REPRESENTATION_RELATIONSHIP()
);
#139=(
REPRESENTATION_RELATIONSHIP($,$,#15418,#15402)
REPRESENTATION_RELATIONSHIP_WITH_TRANSFORMATION(#53)
SHAPE_REPRESENTATION_RELATIONSHIP()
);
#140=(
REPRESENTATION_RELATIONSHIP($,$,#15418,#15402)
REPRESENTATION_RELATIONSHIP_WITH_TRANSFORMATION(#54)
SHAPE_REPRESENTATION_RELATIONSHIP()
);
#141=(
REPRESENTATION_RELATIONSHIP($,$,#15418,#15402)
REPRESENTATION_RELATIONSHIP_WITH_TRANSFORMATION(#55)
SHAPE_REPRESENTATION_RELATIONSHIP()
);
#142=(
REPRESENTATION_RELATIONSHIP($,$,#15419,#15402)
REPRESENTATION_RELATIONSHIP_WITH_TRANSFORMATION(#56)
SHAPE_REPRESENTATION_RELATIONSHIP()
);
#143=(
REPRESENTATION_RELATIONSHIP($,$,#15425,#15402)
REPRESENTATION_RELATIONSHIP_WITH_TRANSFORMATION(#57)
SHAPE_REPRESENTATION_RELATIONSHIP()
);
#144=(
REPRESENTATION_RELATIONSHIP($,$,#15439,#15402)
REPRESENTATION_RELATIONSHIP_WITH_TRANSFORMATION(#58)
SHAPE_REPRESENTATION_RELATIONSHIP()
);
#145=(
REPRESENTATION_RELATIONSHIP($,$,#15439,#15402)
REPRESENTATION_RELATIONSHIP_WITH_TRANSFORMATION(#59)
SHAPE_REPRESENTATION_RELATIONSHIP()
);
#146=(
REPRESENTATION_RELATIONSHIP($,$,#15439,#15402)
REPRESENTATION_RELATIONSHIP_WITH_TRANSFORMATION(#60)
SHAPE_REPRESENTATION_RELATIONSHIP()
);
#147=(
REPRESENTATION_RELATIONSHIP($,$,#15439,#15402)
REPRESENTATION_RELATIONSHIP_WITH_TRANSFORMATION(#61)
SHAPE_REPRESENTATION_RELATIONSHIP()
);
#148=(
REPRESENTATION_RELATIONSHIP($,$,#15439,#15402)
REPRESENTATION_RELATIONSHIP_WITH_TRANSFORMATION(#62)
SHAPE_REPRESENTATION_RELATIONSHIP()
);
#149=(
REPRESENTATION_RELATIONSHIP($,$,#15439,#15402)
REPRESENTATION_RELATIONSHIP_WITH_TRANSFORMATION(#63)
SHAPE_REPRESENTATION_RELATIONSHIP()
);
#150=(
REPRESENTATION_RELATIONSHIP($,$,#15439,#15402)
REPRESENTATION_RELATIONSHIP_WITH_TRANSFORMATION(#64)
SHAPE_REPRESENTATION_RELATIONSHIP()
);
#151=(
REPRESENTATION_RELATIONSHIP($,$,#15439,#15402)
REPRESENTATION_RELATIONSHIP_WITH_TRANSFORMATION(#65)
SHAPE_REPRESENTATION_RELATIONSHIP()
);
#152=(
REPRESENTATION_RELATIONSHIP($,$,#15439,#15402)
REPRESENTATION_RELATIONSHIP_WITH_TRANSFORMATION(#66)
SHAPE_REPRESENTATION_RELATIONSHIP()
);
#153=(
REPRESENTATION_RELATIONSHIP($,$,#15439,#15402)
REPRESENTATION_RELATIONSHIP_WITH_TRANSFORMATION(#67)
SHAPE_REPRESENTATION_RELATIONSHIP()
);
#154=(
REPRESENTATION_RELATIONSHIP($,$,#15439,#15402)
REPRESENTATION_RELATIONSHIP_WITH_TRANSFORMATION(#68)
SHAPE_REPRESENTATION_RELATIONSHIP()
);
#155=(
REPRESENTATION_RELATIONSHIP($,$,#15439,#15402)
REPRESENTATION_RELATIONSHIP_WITH_TRANSFORMATION(#69)
SHAPE_REPRESENTATION_RELATIONSHIP()
);
#156=(
REPRESENTATION_RELATIONSHIP($,$,#15440,#15402)
REPRESENTATION_RELATIONSHIP_WITH_TRANSFORMATION(#70)
SHAPE_REPRESENTATION_RELATIONSHIP()
);
#157=(
REPRESENTATION_RELATIONSHIP($,$,#15440,#15402)
REPRESENTATION_RELATIONSHIP_WITH_TRANSFORMATION(#71)
SHAPE_REPRESENTATION_RELATIONSHIP()
);
#158=(
REPRESENTATION_RELATIONSHIP($,$,#15440,#15402)
REPRESENTATION_RELATIONSHIP_WITH_TRANSFORMATION(#72)
SHAPE_REPRESENTATION_RELATIONSHIP()
);
#159=(
REPRESENTATION_RELATIONSHIP($,$,#15440,#15402)
REPRESENTATION_RELATIONSHIP_WITH_TRANSFORMATION(#73)
SHAPE_REPRESENTATION_RELATIONSHIP()
);
#160=(
REPRESENTATION_RELATIONSHIP($,$,#15428,#15402)
REPRESENTATION_RELATIONSHIP_WITH_TRANSFORMATION(#74)
SHAPE_REPRESENTATION_RELATIONSHIP()
);
#161=(
REPRESENTATION_RELATIONSHIP($,$,#15430,#15429)
REPRESENTATION_RELATIONSHIP_WITH_TRANSFORMATION(#75)
SHAPE_REPRESENTATION_RELATIONSHIP()
);
#162=(
REPRESENTATION_RELATIONSHIP($,$,#15431,#15429)
REPRESENTATION_RELATIONSHIP_WITH_TRANSFORMATION(#76)
SHAPE_REPRESENTATION_RELATIONSHIP()
);
#163=(
REPRESENTATION_RELATIONSHIP($,$,#15432,#15429)
REPRESENTATION_RELATIONSHIP_WITH_TRANSFORMATION(#77)
SHAPE_REPRESENTATION_RELATIONSHIP()
);
#164=(
REPRESENTATION_RELATIONSHIP($,$,#15433,#15429)
REPRESENTATION_RELATIONSHIP_WITH_TRANSFORMATION(#78)
SHAPE_REPRESENTATION_RELATIONSHIP()
);
#165=(
REPRESENTATION_RELATIONSHIP($,$,#15434,#15429)
REPRESENTATION_RELATIONSHIP_WITH_TRANSFORMATION(#79)
SHAPE_REPRESENTATION_RELATIONSHIP()
);
#166=(
REPRESENTATION_RELATIONSHIP($,$,#15435,#15429)
REPRESENTATION_RELATIONSHIP_WITH_TRANSFORMATION(#80)
SHAPE_REPRESENTATION_RELATIONSHIP()
);
#167=(
REPRESENTATION_RELATIONSHIP($,$,#15436,#15429)
REPRESENTATION_RELATIONSHIP_WITH_TRANSFORMATION(#81)
SHAPE_REPRESENTATION_RELATIONSHIP()
);
#168=(
REPRESENTATION_RELATIONSHIP($,$,#15437,#15429)
REPRESENTATION_RELATIONSHIP_WITH_TRANSFORMATION(#82)
SHAPE_REPRESENTATION_RELATIONSHIP()
);
#169=(
REPRESENTATION_RELATIONSHIP($,$,#15438,#15429)
REPRESENTATION_RELATIONSHIP_WITH_TRANSFORMATION(#83)
SHAPE_REPRESENTATION_RELATIONSHIP()
);
#170=(
REPRESENTATION_RELATIONSHIP($,$,#15439,#15429)
REPRESENTATION_RELATIONSHIP_WITH_TRANSFORMATION(#84)
SHAPE_REPRESENTATION_RELATIONSHIP()
);
#171=(
REPRESENTATION_RELATIONSHIP($,$,#15440,#15429)
REPRESENTATION_RELATIONSHIP_WITH_TRANSFORMATION(#85)
SHAPE_REPRESENTATION_RELATIONSHIP()
);
#172=(
REPRESENTATION_RELATIONSHIP($,$,#15442,#15441)
REPRESENTATION_RELATIONSHIP_WITH_TRANSFORMATION(#86)
SHAPE_REPRESENTATION_RELATIONSHIP()
);
#173=(
REPRESENTATION_RELATIONSHIP($,$,#15443,#15441)
REPRESENTATION_RELATIONSHIP_WITH_TRANSFORMATION(#87)
SHAPE_REPRESENTATION_RELATIONSHIP()
);
#174=(
REPRESENTATION_RELATIONSHIP($,$,#15444,#15441)
REPRESENTATION_RELATIONSHIP_WITH_TRANSFORMATION(#88)
SHAPE_REPRESENTATION_RELATIONSHIP()
);
#175=(
REPRESENTATION_RELATIONSHIP($,$,#15446,#15445)
REPRESENTATION_RELATIONSHIP_WITH_TRANSFORMATION(#89)
SHAPE_REPRESENTATION_RELATIONSHIP()
);
#176=(
REPRESENTATION_RELATIONSHIP($,$,#15447,#15445)
REPRESENTATION_RELATIONSHIP_WITH_TRANSFORMATION(#90)
SHAPE_REPRESENTATION_RELATIONSHIP()
);
#177=(
REPRESENTATION_RELATIONSHIP($,$,#15448,#15445)
REPRESENTATION_RELATIONSHIP_WITH_TRANSFORMATION(#91)
SHAPE_REPRESENTATION_RELATIONSHIP()
);
#178=(
REPRESENTATION_RELATIONSHIP($,$,#15449,#15445)
REPRESENTATION_RELATIONSHIP_WITH_TRANSFORMATION(#92)
SHAPE_REPRESENTATION_RELATIONSHIP()
);
#179=(
REPRESENTATION_RELATIONSHIP($,$,#15402,#15401)
REPRESENTATION_RELATIONSHIP_WITH_TRANSFORMATION(#93)
SHAPE_REPRESENTATION_RELATIONSHIP()
);
#180=(
REPRESENTATION_RELATIONSHIP($,$,#15429,#15401)
REPRESENTATION_RELATIONSHIP_WITH_TRANSFORMATION(#94)
SHAPE_REPRESENTATION_RELATIONSHIP()
);
#181=(
REPRESENTATION_RELATIONSHIP($,$,#15441,#15401)
REPRESENTATION_RELATIONSHIP_WITH_TRANSFORMATION(#95)
SHAPE_REPRESENTATION_RELATIONSHIP()
);
#182=(
REPRESENTATION_RELATIONSHIP($,$,#15445,#15401)
REPRESENTATION_RELATIONSHIP_WITH_TRANSFORMATION(#96)
SHAPE_REPRESENTATION_RELATIONSHIP()
);
#183=CONTEXT_DEPENDENT_SHAPE_REPRESENTATION(#97,#15290);
#184=CONTEXT_DEPENDENT_SHAPE_REPRESENTATION(#98,#15291);
#185=CONTEXT_DEPENDENT_SHAPE_REPRESENTATION(#99,#15292);
#186=CONTEXT_DEPENDENT_SHAPE_REPRESENTATION(#100,#15293);
#187=CONTEXT_DEPENDENT_SHAPE_REPRESENTATION(#101,#15294);
#188=CONTEXT_DEPENDENT_SHAPE_REPRESENTATION(#102,#15298);
#189=CONTEXT_DEPENDENT_SHAPE_REPRESENTATION(#103,#15299);
#190=CONTEXT_DEPENDENT_SHAPE_REPRESENTATION(#104,#15313);
#191=CONTEXT_DEPENDENT_SHAPE_REPRESENTATION(#105,#15314);
#192=CONTEXT_DEPENDENT_SHAPE_REPRESENTATION(#106,#15315);
#193=CONTEXT_DEPENDENT_SHAPE_REPRESENTATION(#107,#15316);
#194=CONTEXT_DEPENDENT_SHAPE_REPRESENTATION(#108,#15317);
#195=CONTEXT_DEPENDENT_SHAPE_REPRESENTATION(#109,#15318);
#196=CONTEXT_DEPENDENT_SHAPE_REPRESENTATION(#110,#15319);
#197=CONTEXT_DEPENDENT_SHAPE_REPRESENTATION(#111,#15320);
#198=CONTEXT_DEPENDENT_SHAPE_REPRESENTATION(#112,#15321);
#199=CONTEXT_DEPENDENT_SHAPE_REPRESENTATION(#113,#15322);
#200=CONTEXT_DEPENDENT_SHAPE_REPRESENTATION(#114,#15323);
#201=CONTEXT_DEPENDENT_SHAPE_REPRESENTATION(#115,#15324);
#202=CONTEXT_DEPENDENT_SHAPE_REPRESENTATION(#116,#15325);
#203=CONTEXT_DEPENDENT_SHAPE_REPRESENTATION(#117,#15326);
#204=CONTEXT_DEPENDENT_SHAPE_REPRESENTATION(#118,#15327);
#205=CONTEXT_DEPENDENT_SHAPE_REPRESENTATION(#119,#15328);
#206=CONTEXT_DEPENDENT_SHAPE_REPRESENTATION(#120,#15329);
#207=CONTEXT_DEPENDENT_SHAPE_REPRESENTATION(#121,#15330);
#208=CONTEXT_DEPENDENT_SHAPE_REPRESENTATION(#122,#15331);
#209=CONTEXT_DEPENDENT_SHAPE_REPRESENTATION(#123,#15332);
#210=CONTEXT_DEPENDENT_SHAPE_REPRESENTATION(#124,#15333);
#211=CONTEXT_DEPENDENT_SHAPE_REPRESENTATION(#125,#15334);
#212=CONTEXT_DEPENDENT_SHAPE_REPRESENTATION(#126,#15335);
#213=CONTEXT_DEPENDENT_SHAPE_REPRESENTATION(#127,#15336);
#214=CONTEXT_DEPENDENT_SHAPE_REPRESENTATION(#128,#15337);
#215=CONTEXT_DEPENDENT_SHAPE_REPRESENTATION(#129,#15338);
#216=CONTEXT_DEPENDENT_SHAPE_REPRESENTATION(#130,#15339);
#217=CONTEXT_DEPENDENT_SHAPE_REPRESENTATION(#131,#15340);
#218=CONTEXT_DEPENDENT_SHAPE_REPRESENTATION(#132,#15341);
#219=CONTEXT_DEPENDENT_SHAPE_REPRESENTATION(#133,#15342);
#220=CONTEXT_DEPENDENT_SHAPE_REPRESENTATION(#134,#15343);
#221=CONTEXT_DEPENDENT_SHAPE_REPRESENTATION(#135,#15344);
#222=CONTEXT_DEPENDENT_SHAPE_REPRESENTATION(#136,#15345);
#223=CONTEXT_DEPENDENT_SHAPE_REPRESENTATION(#137,#15346);
#224=CONTEXT_DEPENDENT_SHAPE_REPRESENTATION(#138,#15347);
#225=CONTEXT_DEPENDENT_SHAPE_REPRESENTATION(#139,#15348);
#226=CONTEXT_DEPENDENT_SHAPE_REPRESENTATION(#140,#15349);
#227=CONTEXT_DEPENDENT_SHAPE_REPRESENTATION(#141,#15350);
#228=CONTEXT_DEPENDENT_SHAPE_REPRESENTATION(#142,#15351);
#229=CONTEXT_DEPENDENT_SHAPE_REPRESENTATION(#143,#15352);
#230=CONTEXT_DEPENDENT_SHAPE_REPRESENTATION(#144,#15353);
#231=CONTEXT_DEPENDENT_SHAPE_REPRESENTATION(#145,#15354);
#232=CONTEXT_DEPENDENT_SHAPE_REPRESENTATION(#146,#15355);
#233=CONTEXT_DEPENDENT_SHAPE_REPRESENTATION(#147,#15356);
#234=CONTEXT_DEPENDENT_SHAPE_REPRESENTATION(#148,#15357);
#235=CONTEXT_DEPENDENT_SHAPE_REPRESENTATION(#149,#15358);
#236=CONTEXT_DEPENDENT_SHAPE_REPRESENTATION(#150,#15359);
#237=CONTEXT_DEPENDENT_SHAPE_REPRESENTATION(#151,#15360);
#238=CONTEXT_DEPENDENT_SHAPE_REPRESENTATION(#152,#15361);
#239=CONTEXT_DEPENDENT_SHAPE_REPRESENTATION(#153,#15362);
#240=CONTEXT_DEPENDENT_SHAPE_REPRESENTATION(#154,#15363);
#241=CONTEXT_DEPENDENT_SHAPE_REPRESENTATION(#155,#15364);
#242=CONTEXT_DEPENDENT_SHAPE_REPRESENTATION(#156,#15365);
#243=CONTEXT_DEPENDENT_SHAPE_REPRESENTATION(#157,#15366);
#244=CONTEXT_DEPENDENT_SHAPE_REPRESENTATION(#158,#15367);
#245=CONTEXT_DEPENDENT_SHAPE_REPRESENTATION(#159,#15368);
#246=CONTEXT_DEPENDENT_SHAPE_REPRESENTATION(#160,#15369);
#247=CONTEXT_DEPENDENT_SHAPE_REPRESENTATION(#161,#15370);
#248=CONTEXT_DEPENDENT_SHAPE_REPRESENTATION(#162,#15371);
#249=CONTEXT_DEPENDENT_SHAPE_REPRESENTATION(#163,#15372);
#250=CONTEXT_DEPENDENT_SHAPE_REPRESENTATION(#164,#15373);
#251=CONTEXT_DEPENDENT_SHAPE_REPRESENTATION(#165,#15374);
#252=CONTEXT_DEPENDENT_SHAPE_REPRESENTATION(#166,#15375);
#253=CONTEXT_DEPENDENT_SHAPE_REPRESENTATION(#167,#15376);
#254=CONTEXT_DEPENDENT_SHAPE_REPRESENTATION(#168,#15377);
#255=CONTEXT_DEPENDENT_SHAPE_REPRESENTATION(#169,#15378);
#256=CONTEXT_DEPENDENT_SHAPE_REPRESENTATION(#170,#15379);
#257=CONTEXT_DEPENDENT_SHAPE_REPRESENTATION(#171,#15380);
#258=CONTEXT_DEPENDENT_SHAPE_REPRESENTATION(#172,#15385);
#259=CONTEXT_DEPENDENT_SHAPE_REPRESENTATION(#173,#15386);
#260=CONTEXT_DEPENDENT_SHAPE_REPRESENTATION(#174,#15387);
#261=CONTEXT_DEPENDENT_SHAPE_REPRESENTATION(#175,#15393);
#262=CONTEXT_DEPENDENT_SHAPE_REPRESENTATION(#176,#15394);
#263=CONTEXT_DEPENDENT_SHAPE_REPRESENTATION(#177,#15395);
#264=CONTEXT_DEPENDENT_SHAPE_REPRESENTATION(#178,#15396);
#265=CONTEXT_DEPENDENT_SHAPE_REPRESENTATION(#179,#15397);
#266=CONTEXT_DEPENDENT_SHAPE_REPRESENTATION(#180,#15398);
#267=CONTEXT_DEPENDENT_SHAPE_REPRESENTATION(#181,#15399);
#268=CONTEXT_DEPENDENT_SHAPE_REPRESENTATION(#182,#15400);
#269=NEXT_ASSEMBLY_USAGE_OCCURRENCE('Inner ring:1','Inner ring:1',
'Inner ring:1',#15469,#15470,'Inner ring:1');
#270=NEXT_ASSEMBLY_USAGE_OCCURRENCE('Outer ring:1','Outer ring:1',
'Outer ring:1',#15469,#15471,'Outer ring:1');
#271=NEXT_ASSEMBLY_USAGE_OCCURRENCE('Balls:1','Balls:1','Balls:1',#15469,
#15472,'Balls:1');
#272=NEXT_ASSEMBLY_USAGE_OCCURRENCE('Cage:1','Cage:1','Cage:1',#15469,#15473,
'Cage:1');
#273=NEXT_ASSEMBLY_USAGE_OCCURRENCE('Seals 2RS:1','Seals 2RS:1',
'Seals 2RS:1',#15469,#15474,'Seals 2RS:1');
#274=NEXT_ASSEMBLY_USAGE_OCCURRENCE('Steel sleeve:1','Steel sleeve:1',
'Steel sleeve:1',#15475,#15476,'Steel sleeve:1');
#275=NEXT_ASSEMBLY_USAGE_OCCURRENCE('Ball retainer (plastic):1',
'Ball retainer (plastic):1','Ball retainer (plastic):1',#15475,#15477,
'Ball retainer (plastic):1');
#276=NEXT_ASSEMBLY_USAGE_OCCURRENCE('Base:1','Base:1','Base:1',#15452,#15453,
'Base:1');
#277=NEXT_ASSEMBLY_USAGE_OCCURRENCE('Fixture mounting plate:1',
'Fixture mounting plate:1','Fixture mounting plate:1',#15452,#15454,
'Fixture mounting plate:1');
#278=NEXT_ASSEMBLY_USAGE_OCCURRENCE('Fixture foot strip:1',
'Fixture foot strip:1','Fixture foot strip:1',#15452,#15455,
'Fixture foot strip:1');
#279=NEXT_ASSEMBLY_USAGE_OCCURRENCE('Fixture foot strip (1):1',
'Fixture foot strip (1):1','Fixture foot strip (1):1',#15452,#15456,
'Fixture foot strip (1):1');
#280=NEXT_ASSEMBLY_USAGE_OCCURRENCE('Bearing frame:1','Bearing frame:1',
'Bearing frame:1',#15452,#15457,'Bearing frame:1');
#281=NEXT_ASSEMBLY_USAGE_OCCURRENCE('Front bearing cap:1',
'Front bearing cap:1','Front bearing cap:1',#15452,#15458,
'Front bearing cap:1');
#282=NEXT_ASSEMBLY_USAGE_OCCURRENCE('Rear bearing cap:1',
'Rear bearing cap:1','Rear bearing cap:1',#15452,#15459,
'Rear bearing cap:1');
#283=NEXT_ASSEMBLY_USAGE_OCCURRENCE('Linear bearing cap:1',
'Linear bearing cap:1','Linear bearing cap:1',#15452,#15460,
'Linear bearing cap:1');
#284=NEXT_ASSEMBLY_USAGE_OCCURRENCE('Bar specimen envelope:1',
'Bar specimen envelope:1','Bar specimen envelope:1',#15452,#15461,
'Bar specimen envelope:1');
#285=NEXT_ASSEMBLY_USAGE_OCCURRENCE('Left bar guide:1',
'Left bar guide:1','Left bar guide:1',#15452,#15462,'Left bar guide:1');
#286=NEXT_ASSEMBLY_USAGE_OCCURRENCE('Right bar guide:1',
'Right bar guide:1','Right bar guide:1',#15452,#15463,
'Right bar guide:1');
#287=NEXT_ASSEMBLY_USAGE_OCCURRENCE('Closed lever stop:1',
'Closed lever stop:1','Closed lever stop:1',#15452,#15464,
'Closed lever stop:1');
#288=NEXT_ASSEMBLY_USAGE_OCCURRENCE(
'Slotted Extrusion - 20 x 20 x 200 mm:2',
'Slotted Extrusion - 20 x 20 x 200 mm:2',
'Slotted Extrusion - 20 x 20 x 200 mm:2',#15452,#15465,
'Slotted Extrusion - 20 x 20 x 200 mm:2');
#289=NEXT_ASSEMBLY_USAGE_OCCURRENCE('Captive slot nut:2',
'Captive slot nut:2','Captive slot nut:2',#15452,#15466,
'Captive slot nut:2');
#290=NEXT_ASSEMBLY_USAGE_OCCURRENCE('M5x14 Cap Screw:2',
'M5x14 Cap Screw:2','M5x14 Cap Screw:2',#15452,#15468,
'M5x14 Cap Screw:2');
#291=NEXT_ASSEMBLY_USAGE_OCCURRENCE('Captive slot nut:3',
'Captive slot nut:3','Captive slot nut:3',#15452,#15466,
'Captive slot nut:3');
#292=NEXT_ASSEMBLY_USAGE_OCCURRENCE('Flat Washer - M5:2',
'Flat Washer - M5:2','Flat Washer - M5:2',#15452,#15467,
'Flat Washer - M5:2');
#293=NEXT_ASSEMBLY_USAGE_OCCURRENCE('M5x14 Cap Screw:3',
'M5x14 Cap Screw:3','M5x14 Cap Screw:3',#15452,#15468,
'M5x14 Cap Screw:3');
#294=NEXT_ASSEMBLY_USAGE_OCCURRENCE('Captive slot nut:4',
'Captive slot nut:4','Captive slot nut:4',#15452,#15466,
'Captive slot nut:4');
#295=NEXT_ASSEMBLY_USAGE_OCCURRENCE('M5x14 Cap Screw:4',
'M5x14 Cap Screw:4','M5x14 Cap Screw:4',#15452,#15468,
'M5x14 Cap Screw:4');
#296=NEXT_ASSEMBLY_USAGE_OCCURRENCE('Captive slot nut:5',
'Captive slot nut:5','Captive slot nut:5',#15452,#15466,
'Captive slot nut:5');
#297=NEXT_ASSEMBLY_USAGE_OCCURRENCE('Flat Washer - M5:3',
'Flat Washer - M5:3','Flat Washer - M5:3',#15452,#15467,
'Flat Washer - M5:3');
#298=NEXT_ASSEMBLY_USAGE_OCCURRENCE('M5x14 Cap Screw:5',
'M5x14 Cap Screw:5','M5x14 Cap Screw:5',#15452,#15468,
'M5x14 Cap Screw:5');
#299=NEXT_ASSEMBLY_USAGE_OCCURRENCE(
'Slotted Extrusion - 20 x 20 x 200 mm:3',
'Slotted Extrusion - 20 x 20 x 200 mm:3',
'Slotted Extrusion - 20 x 20 x 200 mm:3',#15452,#15465,
'Slotted Extrusion - 20 x 20 x 200 mm:3');
#300=NEXT_ASSEMBLY_USAGE_OCCURRENCE('Captive slot nut:6',
'Captive slot nut:6','Captive slot nut:6',#15452,#15466,
'Captive slot nut:6');
#301=NEXT_ASSEMBLY_USAGE_OCCURRENCE('M5x14 Cap Screw:6',
'M5x14 Cap Screw:6','M5x14 Cap Screw:6',#15452,#15468,
'M5x14 Cap Screw:6');
#302=NEXT_ASSEMBLY_USAGE_OCCURRENCE('Captive slot nut:7',
'Captive slot nut:7','Captive slot nut:7',#15452,#15466,
'Captive slot nut:7');
#303=NEXT_ASSEMBLY_USAGE_OCCURRENCE('Flat Washer - M5:4',
'Flat Washer - M5:4','Flat Washer - M5:4',#15452,#15467,
'Flat Washer - M5:4');
#304=NEXT_ASSEMBLY_USAGE_OCCURRENCE('M5x14 Cap Screw:7',
'M5x14 Cap Screw:7','M5x14 Cap Screw:7',#15452,#15468,
'M5x14 Cap Screw:7');
#305=NEXT_ASSEMBLY_USAGE_OCCURRENCE('Captive slot nut:8',
'Captive slot nut:8','Captive slot nut:8',#15452,#15466,
'Captive slot nut:8');
#306=NEXT_ASSEMBLY_USAGE_OCCURRENCE('M5x14 Cap Screw:8',
'M5x14 Cap Screw:8','M5x14 Cap Screw:8',#15452,#15468,
'M5x14 Cap Screw:8');
#307=NEXT_ASSEMBLY_USAGE_OCCURRENCE('Captive slot nut:9',
'Captive slot nut:9','Captive slot nut:9',#15452,#15466,
'Captive slot nut:9');
#308=NEXT_ASSEMBLY_USAGE_OCCURRENCE('Flat Washer - M5:5',
'Flat Washer - M5:5','Flat Washer - M5:5',#15452,#15467,
'Flat Washer - M5:5');
#309=NEXT_ASSEMBLY_USAGE_OCCURRENCE('M5x14 Cap Screw:9',
'M5x14 Cap Screw:9','M5x14 Cap Screw:9',#15452,#15468,
'M5x14 Cap Screw:9');
#310=NEXT_ASSEMBLY_USAGE_OCCURRENCE('M5x14 Cap Screw:10',
'M5x14 Cap Screw:10','M5x14 Cap Screw:10',#15452,#15468,
'M5x14 Cap Screw:10');
#311=NEXT_ASSEMBLY_USAGE_OCCURRENCE('M5x14 Cap Screw:11',
'M5x14 Cap Screw:11','M5x14 Cap Screw:11',#15452,#15468,
'M5x14 Cap Screw:11');
#312=NEXT_ASSEMBLY_USAGE_OCCURRENCE('M5x14 Cap Screw:12',
'M5x14 Cap Screw:12','M5x14 Cap Screw:12',#15452,#15468,
'M5x14 Cap Screw:12');
#313=NEXT_ASSEMBLY_USAGE_OCCURRENCE('M5x14 Cap Screw:13',
'M5x14 Cap Screw:13','M5x14 Cap Screw:13',#15452,#15468,
'M5x14 Cap Screw:13');
#314=NEXT_ASSEMBLY_USAGE_OCCURRENCE(
'Sealed Ball Bearing - 10 x 30 x 9 mm:2',
'Sealed Ball Bearing - 10 x 30 x 9 mm:2',
'Sealed Ball Bearing - 10 x 30 x 9 mm:2',#15452,#15469,
'Sealed Ball Bearing - 10 x 30 x 9 mm:2');
#315=NEXT_ASSEMBLY_USAGE_OCCURRENCE(
'Linear Ball Bushing - 12 x 21 x 30 mm:2',
'Linear Ball Bushing - 12 x 21 x 30 mm:2',
'Linear Ball Bushing - 12 x 21 x 30 mm:2',#15452,#15475,
'Linear Ball Bushing - 12 x 21 x 30 mm:2');
#316=NEXT_ASSEMBLY_USAGE_OCCURRENCE('M4x10 Cap Screw:2',
'M4x10 Cap Screw:2','M4x10 Cap Screw:2',#15452,#15489,
'M4x10 Cap Screw:2');
#317=NEXT_ASSEMBLY_USAGE_OCCURRENCE('M4x10 Cap Screw:3',
'M4x10 Cap Screw:3','M4x10 Cap Screw:3',#15452,#15489,
'M4x10 Cap Screw:3');
#318=NEXT_ASSEMBLY_USAGE_OCCURRENCE('M4x10 Cap Screw:4',
'M4x10 Cap Screw:4','M4x10 Cap Screw:4',#15452,#15489,
'M4x10 Cap Screw:4');
#319=NEXT_ASSEMBLY_USAGE_OCCURRENCE('M4x10 Cap Screw:5',
'M4x10 Cap Screw:5','M4x10 Cap Screw:5',#15452,#15489,
'M4x10 Cap Screw:5');
#320=NEXT_ASSEMBLY_USAGE_OCCURRENCE('M4x10 Cap Screw:6',
'M4x10 Cap Screw:6','M4x10 Cap Screw:6',#15452,#15489,
'M4x10 Cap Screw:6');
#321=NEXT_ASSEMBLY_USAGE_OCCURRENCE('M4x10 Cap Screw:7',
'M4x10 Cap Screw:7','M4x10 Cap Screw:7',#15452,#15489,
'M4x10 Cap Screw:7');
#322=NEXT_ASSEMBLY_USAGE_OCCURRENCE('M4x10 Cap Screw:8',
'M4x10 Cap Screw:8','M4x10 Cap Screw:8',#15452,#15489,
'M4x10 Cap Screw:8');
#323=NEXT_ASSEMBLY_USAGE_OCCURRENCE('M4x10 Cap Screw:9',
'M4x10 Cap Screw:9','M4x10 Cap Screw:9',#15452,#15489,
'M4x10 Cap Screw:9');
#324=NEXT_ASSEMBLY_USAGE_OCCURRENCE('M4x10 Cap Screw:10',
'M4x10 Cap Screw:10','M4x10 Cap Screw:10',#15452,#15489,
'M4x10 Cap Screw:10');
#325=NEXT_ASSEMBLY_USAGE_OCCURRENCE('M4x10 Cap Screw:11',
'M4x10 Cap Screw:11','M4x10 Cap Screw:11',#15452,#15489,
'M4x10 Cap Screw:11');
#326=NEXT_ASSEMBLY_USAGE_OCCURRENCE('M4x10 Cap Screw:12',
'M4x10 Cap Screw:12','M4x10 Cap Screw:12',#15452,#15489,
'M4x10 Cap Screw:12');
#327=NEXT_ASSEMBLY_USAGE_OCCURRENCE('M4x10 Cap Screw:13',
'M4x10 Cap Screw:13','M4x10 Cap Screw:13',#15452,#15489,
'M4x10 Cap Screw:13');
#328=NEXT_ASSEMBLY_USAGE_OCCURRENCE('Cap Screw - M4x16:3',
'Cap Screw - M4x16:3','Cap Screw - M4x16:3',#15452,#15490,
'Cap Screw - M4x16:3');
#329=NEXT_ASSEMBLY_USAGE_OCCURRENCE('Cap Screw - M4x16:4',
'Cap Screw - M4x16:4','Cap Screw - M4x16:4',#15452,#15490,
'Cap Screw - M4x16:4');
#330=NEXT_ASSEMBLY_USAGE_OCCURRENCE('Cap Screw - M4x16:5',
'Cap Screw - M4x16:5','Cap Screw - M4x16:5',#15452,#15490,
'Cap Screw - M4x16:5');
#331=NEXT_ASSEMBLY_USAGE_OCCURRENCE('Cap Screw - M4x16:6',
'Cap Screw - M4x16:6','Cap Screw - M4x16:6',#15452,#15490,
'Cap Screw - M4x16:6');
#332=NEXT_ASSEMBLY_USAGE_OCCURRENCE('M4x30 stop screw:2',
'M4x30 stop screw:2','M4x30 stop screw:2',#15452,#15478,
'M4x30 stop screw:2');
#333=NEXT_ASSEMBLY_USAGE_OCCURRENCE('Lever and spindle:1',
'Lever and spindle:1','Lever and spindle:1',#15479,#15480,
'Lever and spindle:1');
#334=NEXT_ASSEMBLY_USAGE_OCCURRENCE('Inner race spacer:1',
'Inner race spacer:1','Inner race spacer:1',#15479,#15481,
'Inner race spacer:1');
#335=NEXT_ASSEMBLY_USAGE_OCCURRENCE('Shaft collar:1','Shaft collar:1',
'Shaft collar:1',#15479,#15482,'Shaft collar:1');
#336=NEXT_ASSEMBLY_USAGE_OCCURRENCE('Lever link pin:1',
'Lever link pin:1','Lever link pin:1',#15479,#15483,'Lever link pin:1');
#337=NEXT_ASSEMBLY_USAGE_OCCURRENCE('Rear pin spacer:1',
'Rear pin spacer:1','Rear pin spacer:1',#15479,#15484,
'Rear pin spacer:1');
#338=NEXT_ASSEMBLY_USAGE_OCCURRENCE('Front pin spacer:1',
'Front pin spacer:1','Front pin spacer:1',#15479,#15485,
'Front pin spacer:1');
#339=NEXT_ASSEMBLY_USAGE_OCCURRENCE('Front pin keeper:1',
'Front pin keeper:1','Front pin keeper:1',#15479,#15486,
'Front pin keeper:1');
#340=NEXT_ASSEMBLY_USAGE_OCCURRENCE('Rear pin keeper:1',
'Rear pin keeper:1','Rear pin keeper:1',#15479,#15487,
'Rear pin keeper:1');
#341=NEXT_ASSEMBLY_USAGE_OCCURRENCE('M4x4 collar screw:2',
'M4x4 collar screw:2','M4x4 collar screw:2',#15479,#15488,
'M4x4 collar screw:2');
#342=NEXT_ASSEMBLY_USAGE_OCCURRENCE('M4x10 Cap Screw:14',
'M4x10 Cap Screw:14','M4x10 Cap Screw:14',#15479,#15489,
'M4x10 Cap Screw:14');
#343=NEXT_ASSEMBLY_USAGE_OCCURRENCE('Cap Screw - M4x16:2',
'Cap Screw - M4x16:2','Cap Screw - M4x16:2',#15479,#15490,
'Cap Screw - M4x16:2');
#344=NEXT_ASSEMBLY_USAGE_OCCURRENCE('Connecting link:1',
'Connecting link:1','Connecting link:1',#15491,#15492,
'Connecting link:1');
#345=NEXT_ASSEMBLY_USAGE_OCCURRENCE('Link bush:1','Link bush:1',
'Link bush:1',#15491,#15493,'Link bush:1');
#346=NEXT_ASSEMBLY_USAGE_OCCURRENCE('Link bush (1):1','Link bush (1):1',
'Link bush (1):1',#15491,#15494,'Link bush (1):1');
#347=NEXT_ASSEMBLY_USAGE_OCCURRENCE('Plunger and fork:1',
'Plunger and fork:1','Plunger and fork:1',#15495,#15496,
'Plunger and fork:1');
#348=NEXT_ASSEMBLY_USAGE_OCCURRENCE('Fork pin:1','Fork pin:1',
'Fork pin:1',#15495,#15497,'Fork pin:1');
#349=NEXT_ASSEMBLY_USAGE_OCCURRENCE(
'Elastomer pressure pad installed:1',
'Elastomer pressure pad installed:1',
'Elastomer pressure pad installed:1',#15495,#15498,
'Elastomer pressure pad installed:1');
#350=NEXT_ASSEMBLY_USAGE_OCCURRENCE('Socket Set Screw - M4x6:2',
'Socket Set Screw - M4x6:2','Socket Set Screw - M4x6:2',#15495,#15499,
'Socket Set Screw - M4x6:2');
#351=NEXT_ASSEMBLY_USAGE_OCCURRENCE('Base and guide:1',
'Base and guide:1','Base and guide:1',#15451,#15452,'Base and guide:1');
#352=NEXT_ASSEMBLY_USAGE_OCCURRENCE('Operating lever:1',
'Operating lever:1','Operating lever:1',#15451,#15479,
'Operating lever:1');
#353=NEXT_ASSEMBLY_USAGE_OCCURRENCE('Connecting link (1):1',
'Connecting link (1):1','Connecting link (1):1',#15451,#15491,
'Connecting link (1):1');
#354=NEXT_ASSEMBLY_USAGE_OCCURRENCE('Pressure plunger:1',
'Pressure plunger:1','Pressure plunger:1',#15451,#15495,
'Pressure plunger:1');
#355=B_SPLINE_CURVE_WITH_KNOTS('',3,(#13605,#13606,#13607,#13608,#13609,
#13610,#13611,#13612,#13613,#13614,#13615,#13616,#13617,#13618,#13619,#13620,
#13621,#13622,#13623,#13624,#13625,#13626),.UNSPECIFIED.,.F.,.F.,(4,2,2,
2,2,2,2,2,2,2,4),(0.0473477652366656,0.126350602536658,0.189525903804987,
0.252701205073317,0.313298422430275,0.373895639787233,0.434492857144191,
0.495090074501149,0.558265375769478,0.621440677037807,0.7004435143378),
 .UNSPECIFIED.);
#356=B_SPLINE_CURVE_WITH_KNOTS('',3,(#13630,#13631,#13632,#13633,#13634,
#13635,#13636,#13637,#13638,#13639,#13640,#13641,#13642,#13643,#13644,#13645,
#13646,#13647,#13648,#13649,#13650,#13651),.UNSPECIFIED.,.F.,.F.,(4,2,2,
2,2,2,2,2,2,2,4),(0.0464897534940957,0.0852567806515119,0.170513561303024,
0.246687263103517,0.308657850341199,0.370628437578881,0.432599024816563,
0.494569612054245,0.570743313854739,0.656000094506251,0.694767121663666),
 .UNSPECIFIED.);
#357=B_SPLINE_CURVE_WITH_KNOTS('',3,(#13657,#13658,#13659,#13660,#13661,
#13662,#13663,#13664,#13665,#13666,#13667,#13668,#13669,#13670,#13671,#13672,
#13673,#13674,#13675,#13676,#13677,#13678),.UNSPECIFIED.,.F.,.F.,(4,2,2,
2,2,2,2,2,2,2,4),(0.0464897534940957,0.0852567806515118,0.170513561303024,
0.246687263103517,0.308657850341199,0.370628437578881,0.432599024816563,
0.494569612054245,0.570743313854738,0.65600009450625,0.694767121663666),
 .UNSPECIFIED.);
#358=B_SPLINE_CURVE_WITH_KNOTS('',3,(#13682,#13683,#13684,#13685,#13686,
#13687,#13688,#13689,#13690,#13691,#13692,#13693,#13694,#13695,#13696,#13697,
#13698,#13699,#13700,#13701,#13702,#13703),.UNSPECIFIED.,.F.,.F.,(4,2,2,
2,2,2,2,2,2,2,4),(0.0464897534940957,0.0852567806515119,0.170513561303024,
0.246687263103517,0.308657850341199,0.370628437578881,0.432599024816563,
0.494569612054245,0.570743313854739,0.656000094506251,0.694767121663666),
 .UNSPECIFIED.);
#359=B_SPLINE_CURVE_WITH_KNOTS('',3,(#13707,#13708,#13709,#13710,#13711,
#13712,#13713,#13714,#13715,#13716,#13717,#13718),.UNSPECIFIED.,.F.,.F.,
(4,2,2,2,2,4),(0.0464897534940957,0.0852567806515119,0.170513561303024,
0.246687263103517,0.308657850341199,0.370628437578881),.UNSPECIFIED.);
#360=B_SPLINE_CURVE_WITH_KNOTS('',3,(#13723,#13724,#13725,#13726,#13727,
#13728,#13729,#13730,#13731,#13732,#13733,#13734),.UNSPECIFIED.,.F.,.F.,
(4,2,2,2,2,4),(0.370628437578881,0.432599024816563,0.494569612054245,0.570743313854738,
0.65600009450625,0.694767121663666),.UNSPECIFIED.);
#361=B_SPLINE_CURVE_WITH_KNOTS('',3,(#13738,#13739,#13740,#13741,#13742,
#13743,#13744,#13745,#13746,#13747,#13748,#13749,#13750,#13751,#13752,#13753,
#13754,#13755,#13756,#13757,#13758,#13759),.UNSPECIFIED.,.F.,.F.,(4,2,2,
2,2,2,2,2,2,2,4),(0.0464897534940957,0.0852567806515121,0.170513561303024,
0.246687263103518,0.308657850341199,0.370628437578881,0.432599024816563,
0.494569612054245,0.570743313854738,0.65600009450625,0.694767121663666),
 .UNSPECIFIED.);
#362=B_SPLINE_CURVE_WITH_KNOTS('',3,(#13763,#13764,#13765,#13766,#13767,
#13768,#13769,#13770,#13771,#13772,#13773,#13774,#13775,#13776,#13777,#13778,
#13779,#13780,#13781,#13782,#13783,#13784),.UNSPECIFIED.,.F.,.F.,(4,2,2,
2,2,2,2,2,2,2,4),(0.0464897534940957,0.0852567806515119,0.170513561303024,
0.246687263103517,0.308657850341199,0.370628437578881,0.432599024816563,
0.494569612054245,0.570743313854738,0.65600009450625,0.694767121663667),
 .UNSPECIFIED.);
#363=B_SPLINE_CURVE_WITH_KNOTS('',3,(#13788,#13789,#13790,#13791,#13792,
#13793,#13794,#13795,#13796,#13797,#13798,#13799,#13800,#13801,#13802,#13803,
#13804,#13805,#13806,#13807,#13808,#13809),.UNSPECIFIED.,.F.,.F.,(4,2,2,
2,2,2,2,2,2,2,4),(0.0464897534940957,0.0852567806515119,0.170513561303024,
0.246687263103517,0.308657850341199,0.370628437578881,0.432599024816563,
0.494569612054245,0.570743313854738,0.65600009450625,0.694767121663666),
 .UNSPECIFIED.);
#364=B_SPLINE_CURVE_WITH_KNOTS('',3,(#13813,#13814,#13815,#13816,#13817,
#13818,#13819,#13820,#13821,#13822,#13823,#13824,#13825,#13826,#13827,#13828,
#13829,#13830,#13831,#13832,#13833,#13834),.UNSPECIFIED.,.F.,.F.,(4,2,2,
2,2,2,2,2,2,2,4),(0.0464897534940957,0.0852567806515119,0.170513561303024,
0.246687263103517,0.308657850341199,0.370628437578881,0.432599024816563,
0.494569612054245,0.570743313854739,0.656000094506251,0.694767121663667),
 .UNSPECIFIED.);
#365=B_SPLINE_CURVE_WITH_KNOTS('',3,(#13842,#13843,#13844,#13845,#13846,
#13847,#13848,#13849,#13850,#13851,#13852,#13853,#13854,#13855,#13856,#13857,
#13858,#13859,#13860,#13861,#13862,#13863),.UNSPECIFIED.,.F.,.F.,(4,2,2,
2,2,2,2,2,2,2,4),(0.0473477652366656,0.126350602536658,0.189525903804987,
0.252701205073316,0.313298422430274,0.373895639787232,0.434492857144191,
0.495090074501149,0.558265375769478,0.621440677037807,0.7004435143378),
 .UNSPECIFIED.);
#366=B_SPLINE_CURVE_WITH_KNOTS('',3,(#13871,#13872,#13873,#13874,#13875,
#13876,#13877,#13878,#13879,#13880,#13881,#13882,#13883,#13884,#13885,#13886,
#13887,#13888,#13889,#13890,#13891,#13892),.UNSPECIFIED.,.F.,.F.,(4,2,2,
2,2,2,2,2,2,2,4),(0.0473477652366656,0.126350602536658,0.189525903804987,
0.252701205073317,0.313298422430275,0.373895639787233,0.434492857144191,
0.495090074501149,0.558265375769478,0.621440677037807,0.7004435143378),
 .UNSPECIFIED.);
#367=B_SPLINE_CURVE_WITH_KNOTS('',3,(#13901,#13902,#13903,#13904,#13905,
#13906,#13907,#13908,#13909,#13910,#13911,#13912),.UNSPECIFIED.,.F.,.F.,
(4,2,2,2,2,4),(0.0473477652366656,0.126350602536658,0.189525903804987,0.252701205073316,
0.313298422430275,0.373895639787233),.UNSPECIFIED.);
#368=B_SPLINE_CURVE_WITH_KNOTS('',3,(#13914,#13915,#13916,#13917,#13918,
#13919,#13920,#13921,#13922,#13923,#13924,#13925),.UNSPECIFIED.,.F.,.F.,
(4,2,2,2,2,4),(0.373895639787233,0.434492857144191,0.495090074501149,0.558265375769478,
0.621440677037807,0.7004435143378),.UNSPECIFIED.);
#369=B_SPLINE_CURVE_WITH_KNOTS('',3,(#13932,#13933,#13934,#13935,#13936,
#13937,#13938,#13939,#13940,#13941,#13942,#13943,#13944,#13945,#13946,#13947,
#13948,#13949,#13950,#13951,#13952,#13953),.UNSPECIFIED.,.F.,.F.,(4,2,2,
2,2,2,2,2,2,2,4),(0.0473477652366656,0.126350602536658,0.189525903804987,
0.252701205073316,0.313298422430275,0.373895639787233,0.434492857144191,
0.495090074501149,0.558265375769478,0.621440677037807,0.7004435143378),
 .UNSPECIFIED.);
#370=B_SPLINE_CURVE_WITH_KNOTS('',3,(#13961,#13962,#13963,#13964,#13965,
#13966,#13967,#13968,#13969,#13970,#13971,#13972,#13973,#13974,#13975,#13976,
#13977,#13978,#13979,#13980,#13981,#13982),.UNSPECIFIED.,.F.,.F.,(4,2,2,
2,2,2,2,2,2,2,4),(0.0473477652366656,0.126350602536658,0.189525903804987,
0.252701205073317,0.313298422430275,0.373895639787233,0.434492857144191,
0.495090074501149,0.558265375769478,0.621440677037807,0.7004435143378),
 .UNSPECIFIED.);
#371=B_SPLINE_CURVE_WITH_KNOTS('',3,(#13990,#13991,#13992,#13993,#13994,
#13995,#13996,#13997,#13998,#13999,#14000,#14001,#14002,#14003,#14004,#14005,
#14006,#14007,#14008,#14009,#14010,#14011),.UNSPECIFIED.,.F.,.F.,(4,2,2,
2,2,2,2,2,2,2,4),(0.0473477652366656,0.126350602536658,0.189525903804987,
0.252701205073316,0.313298422430275,0.373895639787233,0.434492857144191,
0.495090074501149,0.558265375769478,0.621440677037807,0.7004435143378),
 .UNSPECIFIED.);
#372=B_SPLINE_CURVE_WITH_KNOTS('',3,(#14020,#14021,#14022,#14023,#14024,
#14025,#14026,#14027,#14028,#14029,#14030,#14031,#14032,#14033,#14034,#14035,
#14036,#14037,#14038,#14039,#14040,#14041),.UNSPECIFIED.,.F.,.F.,(4,2,2,
2,2,2,2,2,2,2,4),(0.0473477652366656,0.126350602536658,0.189525903804987,
0.252701205073317,0.313298422430275,0.373895639787233,0.434492857144191,
0.495090074501149,0.558265375769478,0.621440677037807,0.7004435143378),
 .UNSPECIFIED.);
#373=B_SPLINE_CURVE_WITH_KNOTS('',3,(#14378,#14379,#14380,#14381,#14382,
#14383,#14384,#14385,#14386,#14387,#14388,#14389,#14390,#14391),
 .UNSPECIFIED.,.F.,.F.,(4,2,2,2,2,2,4),(0.618551524396288,0.626563103102763,
0.689203386094986,0.751843669087208,0.814483952079431,0.877124235071654,
0.88513581377813),.UNSPECIFIED.);
#374=B_SPLINE_CURVE_WITH_KNOTS('',3,(#14397,#14398,#14399,#14400,#14401,
#14402,#14403,#14404,#14405,#14406,#14407,#14408,#14409,#14410,#14411,#14412,
#14413,#14414),.UNSPECIFIED.,.F.,.F.,(4,2,2,2,2,2,2,2,4),(0.,0.0623062782223138,
0.124612556444628,0.186916384615148,0.249220212785668,0.311524040956189,
0.373827869126709,0.436134147349023,0.498440425571337),.UNSPECIFIED.);
#375=B_SPLINE_CURVE_WITH_KNOTS('',3,(#14415,#14416,#14417,#14418,#14419,
#14420,#14421,#14422,#14423,#14424,#14425,#14426,#14427,#14428,#14429,#14430,
#14431,#14432),.UNSPECIFIED.,.F.,.F.,(4,2,2,2,2,2,2,2,4),(0.498440425571337,
0.560746703793651,0.623052982015964,0.685356810186485,0.747660638357005,
0.809964466527525,0.872268294698046,0.93457457292036,0.996880851142673),
 .UNSPECIFIED.);
#376=B_SPLINE_CURVE_WITH_KNOTS('',3,(#14435,#14436,#14437,#14438,#14439,
#14440,#14441,#14442,#14443,#14444,#14445,#14446,#14447,#14448),
 .UNSPECIFIED.,.F.,.F.,(4,2,2,2,2,2,4),(0.117322411671483,0.125333990377957,
0.18797427337018,0.250614556362403,0.313254839354626,0.375895122346849,
0.383906701053325),.UNSPECIFIED.);
#377=B_SPLINE_CURVE_WITH_KNOTS('',3,(#14965,#14966,#14967,#14968,#14969,
#14970,#14971,#14972,#14973,#14974),.UNSPECIFIED.,.F.,.F.,(4,2,2,2,4),(0.66642709076087,
0.700624974512804,0.764181514210609,0.827738053908413,0.861935937660348),
 .UNSPECIFIED.);
#378=B_SPLINE_CURVE_WITH_KNOTS('',3,(#14982,#14983,#14984,#14985,#14986,
#14987,#14988,#14989,#14990,#14991),.UNSPECIFIED.,.F.,.F.,(4,2,2,2,4),(0.156972747953797,
0.191170631705732,0.254727171403536,0.318283711101341,0.352481594853276),
 .UNSPECIFIED.);
#379=SPHERICAL_SURFACE('',#9206,0.23815);
#380=SPHERICAL_SURFACE('',#9208,0.23815);
#381=SPHERICAL_SURFACE('',#9210,0.23815);
#382=SPHERICAL_SURFACE('',#9212,0.23815);
#383=SPHERICAL_SURFACE('',#9214,0.23815);
#384=SPHERICAL_SURFACE('',#9216,0.23815);
#385=SPHERICAL_SURFACE('',#9218,0.23815);
#386=SPHERICAL_SURFACE('',#9220,0.23815);
#387=SPHERICAL_SURFACE('',#9223,0.247676);
#388=SPHERICAL_SURFACE('',#9239,0.247676);
#389=SPHERICAL_SURFACE('',#9244,0.247676);
#390=SPHERICAL_SURFACE('',#9249,0.247676);
#391=SPHERICAL_SURFACE('',#9254,0.247676);
#392=SPHERICAL_SURFACE('',#9259,0.247676);
#393=SPHERICAL_SURFACE('',#9264,0.247676);
#394=SPHERICAL_SURFACE('',#9272,0.247676);
#395=TOROIDAL_SURFACE('',#9166,1.,0.247676);
#396=TOROIDAL_SURFACE('',#9186,1.,0.247676);
#397=ORIENTED_CLOSED_SHELL('',*,#8260,.F.);
#398=ORIENTED_CLOSED_SHELL('',*,#8277,.F.);
#399=ORIENTED_CLOSED_SHELL('',*,#8288,.F.);
#400=ORIENTED_CLOSED_SHELL('',*,#8291,.F.);
#401=BREP_WITH_VOIDS('Body1',#8261,(#397));
#402=BREP_WITH_VOIDS('Body1',#8278,(#398));
#403=BREP_WITH_VOIDS('Body1',#8289,(#399));
#404=BREP_WITH_VOIDS('Body1',#8290,(#400));
#405=CONICAL_SURFACE('',#9130,0.275,0.785398163397449);
#406=CONICAL_SURFACE('',#9153,0.4,0.785398163397448);
#407=CONICAL_SURFACE('',#9157,0.41,0.785398163397448);
#408=CONICAL_SURFACE('',#9161,0.26,0.463647609000806);
#409=CONICAL_SURFACE('',#9177,0.53,0.785398163397448);
#410=CONICAL_SURFACE('',#9184,0.53,0.785398163397448);
#411=CONICAL_SURFACE('',#9197,1.47,0.785398163397449);
#412=CONICAL_SURFACE('',#9201,1.47,0.785398163397449);
#413=CONICAL_SURFACE('',#9367,0.325,0.785398163397448);
#414=CONICAL_SURFACE('',#9371,0.335,0.785398163397448);
#415=CONICAL_SURFACE('',#9375,0.21,0.463647609000806);
#416=CONICAL_SURFACE('',#9379,0.18,0.785398163397448);
#417=CONICAL_SURFACE('',#9512,0.185,0.785398163397449);
#418=CONICAL_SURFACE('',#9528,0.325,0.785398163397448);
#419=CONICAL_SURFACE('',#9532,0.335,0.785398163397448);
#420=CONICAL_SURFACE('',#9536,0.21,0.463647609000806);
#421=CONICAL_SURFACE('',#9542,0.325,0.785398163397448);
#422=CONICAL_SURFACE('',#9546,0.335,0.785398163397448);
#423=CONICAL_SURFACE('',#9550,0.21,0.463647609000806);
#424=CONICAL_SURFACE('',#9554,0.18,0.785398163397448);
#425=CONICAL_SURFACE('',#9739,0.185,0.785398163397449);
#426=CONICAL_SURFACE('',#9743,0.1625,0.785398163397449);
#427=ELLIPSE('',#9119,0.299389011154384,0.2117);
#428=ELLIPSE('',#9123,0.299389011154384,0.2117);
#429=SHAPE_REPRESENTATION_RELATIONSHIP('SRR','None',#15403,#471);
#430=SHAPE_REPRESENTATION_RELATIONSHIP('SRR','None',#15404,#472);
#431=SHAPE_REPRESENTATION_RELATIONSHIP('SRR','None',#15405,#473);
#432=SHAPE_REPRESENTATION_RELATIONSHIP('SRR','None',#15406,#474);
#433=SHAPE_REPRESENTATION_RELATIONSHIP('SRR','None',#15407,#475);
#434=SHAPE_REPRESENTATION_RELATIONSHIP('SRR','None',#15408,#476);
#435=SHAPE_REPRESENTATION_RELATIONSHIP('SRR','None',#15409,#477);
#436=SHAPE_REPRESENTATION_RELATIONSHIP('SRR','None',#15410,#478);
#437=SHAPE_REPRESENTATION_RELATIONSHIP('SRR','None',#15411,#479);
#438=SHAPE_REPRESENTATION_RELATIONSHIP('SRR','None',#15412,#480);
#439=SHAPE_REPRESENTATION_RELATIONSHIP('SRR','None',#15413,#481);
#440=SHAPE_REPRESENTATION_RELATIONSHIP('SRR','None',#15414,#482);
#441=SHAPE_REPRESENTATION_RELATIONSHIP('SRR','None',#15415,#483);
#442=SHAPE_REPRESENTATION_RELATIONSHIP('SRR','None',#15416,#484);
#443=SHAPE_REPRESENTATION_RELATIONSHIP('SRR','None',#15417,#485);
#444=SHAPE_REPRESENTATION_RELATIONSHIP('SRR','None',#15418,#486);
#445=SHAPE_REPRESENTATION_RELATIONSHIP('SRR','None',#15420,#487);
#446=SHAPE_REPRESENTATION_RELATIONSHIP('SRR','None',#15421,#488);
#447=SHAPE_REPRESENTATION_RELATIONSHIP('SRR','None',#15422,#489);
#448=SHAPE_REPRESENTATION_RELATIONSHIP('SRR','None',#15423,#490);
#449=SHAPE_REPRESENTATION_RELATIONSHIP('SRR','None',#15424,#491);
#450=SHAPE_REPRESENTATION_RELATIONSHIP('SRR','None',#15426,#492);
#451=SHAPE_REPRESENTATION_RELATIONSHIP('SRR','None',#15427,#493);
#452=SHAPE_REPRESENTATION_RELATIONSHIP('SRR','None',#15428,#494);
#453=SHAPE_REPRESENTATION_RELATIONSHIP('SRR','None',#15430,#495);
#454=SHAPE_REPRESENTATION_RELATIONSHIP('SRR','None',#15431,#496);
#455=SHAPE_REPRESENTATION_RELATIONSHIP('SRR','None',#15432,#497);
#456=SHAPE_REPRESENTATION_RELATIONSHIP('SRR','None',#15433,#498);
#457=SHAPE_REPRESENTATION_RELATIONSHIP('SRR','None',#15434,#499);
#458=SHAPE_REPRESENTATION_RELATIONSHIP('SRR','None',#15435,#500);
#459=SHAPE_REPRESENTATION_RELATIONSHIP('SRR','None',#15436,#501);
#460=SHAPE_REPRESENTATION_RELATIONSHIP('SRR','None',#15437,#502);
#461=SHAPE_REPRESENTATION_RELATIONSHIP('SRR','None',#15438,#503);
#462=SHAPE_REPRESENTATION_RELATIONSHIP('SRR','None',#15439,#504);
#463=SHAPE_REPRESENTATION_RELATIONSHIP('SRR','None',#15440,#505);
#464=SHAPE_REPRESENTATION_RELATIONSHIP('SRR','None',#15442,#506);
#465=SHAPE_REPRESENTATION_RELATIONSHIP('SRR','None',#15443,#507);
#466=SHAPE_REPRESENTATION_RELATIONSHIP('SRR','None',#15444,#508);
#467=SHAPE_REPRESENTATION_RELATIONSHIP('SRR','None',#15446,#509);
#468=SHAPE_REPRESENTATION_RELATIONSHIP('SRR','None',#15447,#510);
#469=SHAPE_REPRESENTATION_RELATIONSHIP('SRR','None',#15448,#511);
#470=SHAPE_REPRESENTATION_RELATIONSHIP('SRR','None',#15449,#512);
#471=ADVANCED_BREP_SHAPE_REPRESENTATION('',(#564),#15165);
#472=ADVANCED_BREP_SHAPE_REPRESENTATION('',(#565),#15166);
#473=ADVANCED_BREP_SHAPE_REPRESENTATION('',(#566),#15167);
#474=ADVANCED_BREP_SHAPE_REPRESENTATION('',(#567),#15168);
#475=ADVANCED_BREP_SHAPE_REPRESENTATION('',(#568),#15169);
#476=ADVANCED_BREP_SHAPE_REPRESENTATION('',(#569),#15170);
#477=ADVANCED_BREP_SHAPE_REPRESENTATION('',(#570),#15171);
#478=ADVANCED_BREP_SHAPE_REPRESENTATION('',(#571),#15172);
#479=ADVANCED_BREP_SHAPE_REPRESENTATION('',(#572),#15173);
#480=ADVANCED_BREP_SHAPE_REPRESENTATION('',(#573),#15174);
#481=ADVANCED_BREP_SHAPE_REPRESENTATION('',(#574),#15175);
#482=ADVANCED_BREP_SHAPE_REPRESENTATION('',(#575),#15176);
#483=ADVANCED_BREP_SHAPE_REPRESENTATION('',(#576),#15177);
#484=ADVANCED_BREP_SHAPE_REPRESENTATION('',(#577),#15178);
#485=ADVANCED_BREP_SHAPE_REPRESENTATION('',(#578),#15179);
#486=ADVANCED_BREP_SHAPE_REPRESENTATION('',(#401),#15180);
#487=ADVANCED_BREP_SHAPE_REPRESENTATION('',(#579),#15182);
#488=ADVANCED_BREP_SHAPE_REPRESENTATION('',(#580),#15183);
#489=ADVANCED_BREP_SHAPE_REPRESENTATION('',(#581,#582,#583,#584,#585,#586,
#587,#588),#15184);
#490=ADVANCED_BREP_SHAPE_REPRESENTATION('',(#589),#15185);
#491=ADVANCED_BREP_SHAPE_REPRESENTATION('',(#590,#591),#15186);
#492=ADVANCED_BREP_SHAPE_REPRESENTATION('',(#592),#15188);
#493=ADVANCED_BREP_SHAPE_REPRESENTATION('',(#593),#15189);
#494=ADVANCED_BREP_SHAPE_REPRESENTATION('',(#402),#15190);
#495=ADVANCED_BREP_SHAPE_REPRESENTATION('',(#594),#15192);
#496=ADVANCED_BREP_SHAPE_REPRESENTATION('',(#595),#15193);
#497=ADVANCED_BREP_SHAPE_REPRESENTATION('',(#596),#15194);
#498=ADVANCED_BREP_SHAPE_REPRESENTATION('',(#597),#15195);
#499=ADVANCED_BREP_SHAPE_REPRESENTATION('',(#598),#15196);
#500=ADVANCED_BREP_SHAPE_REPRESENTATION('',(#599),#15197);
#501=ADVANCED_BREP_SHAPE_REPRESENTATION('',(#600),#15198);
#502=ADVANCED_BREP_SHAPE_REPRESENTATION('',(#601),#15199);
#503=ADVANCED_BREP_SHAPE_REPRESENTATION('',(#602),#15200);
#504=ADVANCED_BREP_SHAPE_REPRESENTATION('',(#403),#15201);
#505=ADVANCED_BREP_SHAPE_REPRESENTATION('',(#404),#15202);
#506=ADVANCED_BREP_SHAPE_REPRESENTATION('',(#603),#15204);
#507=ADVANCED_BREP_SHAPE_REPRESENTATION('',(#604),#15205);
#508=ADVANCED_BREP_SHAPE_REPRESENTATION('',(#605),#15206);
#509=ADVANCED_BREP_SHAPE_REPRESENTATION('',(#606,#607),#15208);
#510=ADVANCED_BREP_SHAPE_REPRESENTATION('',(#608),#15209);
#511=ADVANCED_BREP_SHAPE_REPRESENTATION('',(#609),#15210);
#512=ADVANCED_BREP_SHAPE_REPRESENTATION('',(#610),#15211);
#513=STYLED_ITEM('',(#15698),#564);
#514=STYLED_ITEM('',(#15712),#565);
#515=STYLED_ITEM('',(#15733),#566);
#516=STYLED_ITEM('',(#15733),#567);
#517=STYLED_ITEM('',(#15719),#568);
#518=STYLED_ITEM('',(#15719),#569);
#519=STYLED_ITEM('',(#15719),#570);
#520=STYLED_ITEM('',(#15719),#571);
#521=STYLED_ITEM('',(#15733),#572);
#522=STYLED_ITEM('',(#15712),#573);
#523=STYLED_ITEM('',(#15733),#574);
#524=STYLED_ITEM('',(#15712),#575);
#525=STYLED_ITEM('',(#15733),#576);
#526=STYLED_ITEM('',(#15726),#577);
#527=STYLED_ITEM('',(#15726),#578);
#528=STYLED_ITEM('',(#15726),#401);
#529=STYLED_ITEM('',(#15719),#579);
#530=STYLED_ITEM('',(#15719),#580);
#531=STYLED_ITEM('',(#15719),#581);
#532=STYLED_ITEM('',(#15719),#582);
#533=STYLED_ITEM('',(#15719),#583);
#534=STYLED_ITEM('',(#15719),#584);
#535=STYLED_ITEM('',(#15719),#585);
#536=STYLED_ITEM('',(#15719),#586);
#537=STYLED_ITEM('',(#15719),#587);
#538=STYLED_ITEM('',(#15719),#588);
#539=STYLED_ITEM('',(#15719),#589);
#540=STYLED_ITEM('',(#15719),#590);
#541=STYLED_ITEM('',(#15719),#591);
#542=STYLED_ITEM('',(#15733),#592);
#543=STYLED_ITEM('',(#15712),#593);
#544=STYLED_ITEM('',(#15726),#402);
#545=STYLED_ITEM('',(#15712),#594);
#546=STYLED_ITEM('',(#15719),#595);
#547=STYLED_ITEM('',(#15719),#596);
#548=STYLED_ITEM('',(#15719),#597);
#549=STYLED_ITEM('',(#15719),#598);
#550=STYLED_ITEM('',(#15719),#599);
#551=STYLED_ITEM('',(#15719),#600);
#552=STYLED_ITEM('',(#15719),#601);
#553=STYLED_ITEM('',(#15726),#602);
#554=STYLED_ITEM('',(#15726),#403);
#555=STYLED_ITEM('',(#15726),#404);
#556=STYLED_ITEM('',(#15712),#603);
#557=STYLED_ITEM('',(#15733),#604);
#558=STYLED_ITEM('',(#15733),#605);
#559=STYLED_ITEM('',(#15733),#606);
#560=STYLED_ITEM('',(#15733),#607);
#561=STYLED_ITEM('',(#15719),#608);
#562=STYLED_ITEM('',(#15733),#609);
#563=STYLED_ITEM('',(#15726),#610);
#564=MANIFOLD_SOLID_BREP('Body1',#8245);
#565=MANIFOLD_SOLID_BREP('Body1',#8246);
#566=MANIFOLD_SOLID_BREP('Body1',#8247);
#567=MANIFOLD_SOLID_BREP('Body1',#8248);
#568=MANIFOLD_SOLID_BREP('Body1',#8249);
#569=MANIFOLD_SOLID_BREP('Body1',#8250);
#570=MANIFOLD_SOLID_BREP('Body1',#8251);
#571=MANIFOLD_SOLID_BREP('Body1',#8252);
#572=MANIFOLD_SOLID_BREP('Body1',#8253);
#573=MANIFOLD_SOLID_BREP('Body1',#8254);
#574=MANIFOLD_SOLID_BREP('Body1',#8255);
#575=MANIFOLD_SOLID_BREP('Body1',#8256);
#576=MANIFOLD_SOLID_BREP('Body1',#8257);
#577=MANIFOLD_SOLID_BREP('Body1',#8258);
#578=MANIFOLD_SOLID_BREP('Body1',#8259);
#579=MANIFOLD_SOLID_BREP('Body1',#8262);
#580=MANIFOLD_SOLID_BREP('Body1',#8263);
#581=MANIFOLD_SOLID_BREP('Body1',#8264);
#582=MANIFOLD_SOLID_BREP('Body2',#8265);
#583=MANIFOLD_SOLID_BREP('Body3',#8266);
#584=MANIFOLD_SOLID_BREP('Body4',#8267);
#585=MANIFOLD_SOLID_BREP('Body5',#8268);
#586=MANIFOLD_SOLID_BREP('Body6',#8269);
#587=MANIFOLD_SOLID_BREP('Body7',#8270);
#588=MANIFOLD_SOLID_BREP('Body8',#8271);
#589=MANIFOLD_SOLID_BREP('Continuous crown cage',#8272);
#590=MANIFOLD_SOLID_BREP('Body1',#8273);
#591=MANIFOLD_SOLID_BREP('Body2',#8274);
#592=MANIFOLD_SOLID_BREP('Body1',#8275);
#593=MANIFOLD_SOLID_BREP('Body1',#8276);
#594=MANIFOLD_SOLID_BREP('Body1',#8279);
#595=MANIFOLD_SOLID_BREP('Body1',#8280);
#596=MANIFOLD_SOLID_BREP('Body1',#8281);
#597=MANIFOLD_SOLID_BREP('Body1',#8282);
#598=MANIFOLD_SOLID_BREP('Body1',#8283);
#599=MANIFOLD_SOLID_BREP('Body1',#8284);
#600=MANIFOLD_SOLID_BREP('Body1',#8285);
#601=MANIFOLD_SOLID_BREP('Body1',#8286);
#602=MANIFOLD_SOLID_BREP('Body1',#8287);
#603=MANIFOLD_SOLID_BREP('Body1',#8292);
#604=MANIFOLD_SOLID_BREP('Body1',#8293);
#605=MANIFOLD_SOLID_BREP('Body1',#8294);
#606=MANIFOLD_SOLID_BREP('Body1',#8295);
#607=MANIFOLD_SOLID_BREP('Body2',#8296);
#608=MANIFOLD_SOLID_BREP('Body1',#8297);
#609=MANIFOLD_SOLID_BREP('Body1',#8298);
#610=MANIFOLD_SOLID_BREP('Body1',#8299);
#611=FACE_BOUND('',#1590,.T.);
#612=FACE_BOUND('',#1591,.T.);
#613=FACE_BOUND('',#1592,.T.);
#614=FACE_BOUND('',#1593,.T.);
#615=FACE_BOUND('',#1594,.T.);
#616=FACE_BOUND('',#1595,.T.);
#617=FACE_BOUND('',#1596,.T.);
#618=FACE_BOUND('',#1597,.T.);
#619=FACE_BOUND('',#1598,.T.);
#620=FACE_BOUND('',#1599,.T.);
#621=FACE_BOUND('',#1600,.T.);
#622=FACE_BOUND('',#1601,.T.);
#623=FACE_BOUND('',#1603,.T.);
#624=FACE_BOUND('',#1604,.T.);
#625=FACE_BOUND('',#1605,.T.);
#626=FACE_BOUND('',#1606,.T.);
#627=FACE_BOUND('',#1607,.T.);
#628=FACE_BOUND('',#1608,.T.);
#629=FACE_BOUND('',#1609,.T.);
#630=FACE_BOUND('',#1610,.T.);
#631=FACE_BOUND('',#1611,.T.);
#632=FACE_BOUND('',#1612,.T.);
#633=FACE_BOUND('',#1613,.T.);
#634=FACE_BOUND('',#1614,.T.);
#635=FACE_BOUND('',#1624,.T.);
#636=FACE_BOUND('',#1625,.T.);
#637=FACE_BOUND('',#1626,.T.);
#638=FACE_BOUND('',#1627,.T.);
#639=FACE_BOUND('',#1629,.T.);
#640=FACE_BOUND('',#1630,.T.);
#641=FACE_BOUND('',#1631,.T.);
#642=FACE_BOUND('',#1632,.T.);
#643=FACE_BOUND('',#1664,.T.);
#644=FACE_BOUND('',#1669,.T.);
#645=FACE_BOUND('',#1670,.T.);
#646=FACE_BOUND('',#1671,.T.);
#647=FACE_BOUND('',#1672,.T.);
#648=FACE_BOUND('',#1673,.T.);
#649=FACE_BOUND('',#1674,.T.);
#650=FACE_BOUND('',#1676,.T.);
#651=FACE_BOUND('',#1677,.T.);
#652=FACE_BOUND('',#1678,.T.);
#653=FACE_BOUND('',#1679,.T.);
#654=FACE_BOUND('',#1680,.T.);
#655=FACE_BOUND('',#1682,.T.);
#656=FACE_BOUND('',#1683,.T.);
#657=FACE_BOUND('',#1684,.T.);
#658=FACE_BOUND('',#1685,.T.);
#659=FACE_BOUND('',#1686,.T.);
#660=FACE_BOUND('',#1694,.T.);
#661=FACE_BOUND('',#1695,.T.);
#662=FACE_BOUND('',#1696,.T.);
#663=FACE_BOUND('',#1697,.T.);
#664=FACE_BOUND('',#1698,.T.);
#665=FACE_BOUND('',#1699,.T.);
#666=FACE_BOUND('',#1702,.T.);
#667=FACE_BOUND('',#1707,.T.);
#668=FACE_BOUND('',#1708,.T.);
#669=FACE_BOUND('',#1709,.T.);
#670=FACE_BOUND('',#1710,.T.);
#671=FACE_BOUND('',#1717,.T.);
#672=FACE_BOUND('',#1721,.T.);
#673=FACE_BOUND('',#1722,.T.);
#674=FACE_BOUND('',#1723,.T.);
#675=FACE_BOUND('',#1724,.T.);
#676=FACE_BOUND('',#1725,.T.);
#677=FACE_BOUND('',#1727,.T.);
#678=FACE_BOUND('',#1728,.T.);
#679=FACE_BOUND('',#1729,.T.);
#680=FACE_BOUND('',#1730,.T.);
#681=FACE_BOUND('',#1731,.T.);
#682=FACE_BOUND('',#1738,.T.);
#683=FACE_BOUND('',#1742,.T.);
#684=FACE_BOUND('',#1743,.T.);
#685=FACE_BOUND('',#1744,.T.);
#686=FACE_BOUND('',#1745,.T.);
#687=FACE_BOUND('',#1746,.T.);
#688=FACE_BOUND('',#1748,.T.);
#689=FACE_BOUND('',#1749,.T.);
#690=FACE_BOUND('',#1750,.T.);
#691=FACE_BOUND('',#1751,.T.);
#692=FACE_BOUND('',#1752,.T.);
#693=FACE_BOUND('',#1755,.T.);
#694=FACE_BOUND('',#1758,.T.);
#695=FACE_BOUND('',#1761,.T.);
#696=FACE_BOUND('',#1764,.T.);
#697=FACE_BOUND('',#1771,.T.);
#698=FACE_BOUND('',#1775,.T.);
#699=FACE_BOUND('',#1776,.T.);
#700=FACE_BOUND('',#1777,.T.);
#701=FACE_BOUND('',#1778,.T.);
#702=FACE_BOUND('',#1779,.T.);
#703=FACE_BOUND('',#1781,.T.);
#704=FACE_BOUND('',#1782,.T.);
#705=FACE_BOUND('',#1783,.T.);
#706=FACE_BOUND('',#1784,.T.);
#707=FACE_BOUND('',#1785,.T.);
#708=FACE_BOUND('',#1802,.T.);
#709=FACE_BOUND('',#1803,.T.);
#710=FACE_BOUND('',#1814,.T.);
#711=FACE_BOUND('',#1815,.T.);
#712=FACE_BOUND('',#1819,.T.);
#713=FACE_BOUND('',#1822,.T.);
#714=FACE_BOUND('',#1871,.T.);
#715=FACE_BOUND('',#1873,.T.);
#716=FACE_BOUND('',#1877,.T.);
#717=FACE_BOUND('',#1892,.T.);
#718=FACE_BOUND('',#1895,.T.);
#719=FACE_BOUND('',#1910,.T.);
#720=FACE_BOUND('',#1918,.T.);
#721=FACE_BOUND('',#1921,.T.);
#722=FACE_BOUND('',#1926,.T.);
#723=FACE_BOUND('',#1931,.T.);
#724=FACE_BOUND('',#1959,.T.);
#725=FACE_BOUND('',#1962,.T.);
#726=FACE_BOUND('',#1965,.T.);
#727=FACE_BOUND('',#1968,.T.);
#728=FACE_BOUND('',#1971,.T.);
#729=FACE_BOUND('',#1979,.T.);
#730=FACE_BOUND('',#1982,.T.);
#731=FACE_BOUND('',#1985,.T.);
#732=FACE_BOUND('',#1988,.T.);
#733=FACE_BOUND('',#1991,.T.);
#734=FACE_BOUND('',#1994,.T.);
#735=FACE_BOUND('',#1996,.T.);
#736=FACE_BOUND('',#2002,.T.);
#737=FACE_BOUND('',#2004,.T.);
#738=FACE_BOUND('',#2006,.T.);
#739=FACE_BOUND('',#2008,.T.);
#740=FACE_BOUND('',#2018,.T.);
#741=FACE_BOUND('',#2026,.T.);
#742=FACE_BOUND('',#2033,.T.);
#743=FACE_BOUND('',#2034,.T.);
#744=FACE_BOUND('',#2041,.T.);
#745=FACE_BOUND('',#2044,.T.);
#746=FACE_BOUND('',#2047,.T.);
#747=FACE_BOUND('',#2056,.T.);
#748=FACE_BOUND('',#2058,.T.);
#749=FACE_BOUND('',#2063,.T.);
#750=FACE_BOUND('',#2065,.T.);
#751=FACE_BOUND('',#2067,.T.);
#752=FACE_BOUND('',#2069,.T.);
#753=FACE_BOUND('',#2075,.T.);
#754=FACE_BOUND('',#2077,.T.);
#755=FACE_BOUND('',#2082,.T.);
#756=FACE_BOUND('',#2084,.T.);
#757=FACE_BOUND('',#2088,.T.);
#758=FACE_BOUND('',#2090,.T.);
#759=FACE_BOUND('',#2094,.T.);
#760=FACE_BOUND('',#2096,.T.);
#761=FACE_BOUND('',#2100,.T.);
#762=FACE_BOUND('',#2102,.T.);
#763=FACE_BOUND('',#2106,.T.);
#764=FACE_BOUND('',#2108,.T.);
#765=FACE_BOUND('',#2118,.T.);
#766=FACE_BOUND('',#2135,.T.);
#767=FACE_BOUND('',#2143,.T.);
#768=FACE_BOUND('',#2161,.T.);
#769=FACE_BOUND('',#2162,.T.);
#770=FACE_BOUND('',#2166,.T.);
#771=FACE_BOUND('',#2167,.T.);
#772=FACE_BOUND('',#2171,.T.);
#773=FACE_BOUND('',#2173,.T.);
#774=FACE_BOUND('',#2177,.T.);
#775=FACE_BOUND('',#2179,.T.);
#776=FACE_BOUND('',#2183,.T.);
#777=FACE_BOUND('',#2199,.T.);
#778=FACE_BOUND('',#2201,.T.);
#779=FACE_BOUND('',#2206,.T.);
#780=FACE_BOUND('',#2208,.T.);
#781=FACE_BOUND('',#2210,.T.);
#782=FACE_BOUND('',#2226,.T.);
#783=PLANE('',#8802);
#784=PLANE('',#8803);
#785=PLANE('',#8804);
#786=PLANE('',#8805);
#787=PLANE('',#8806);
#788=PLANE('',#8807);
#789=PLANE('',#8821);
#790=PLANE('',#8822);
#791=PLANE('',#8823);
#792=PLANE('',#8824);
#793=PLANE('',#8825);
#794=PLANE('',#8826);
#795=PLANE('',#8828);
#796=PLANE('',#8829);
#797=PLANE('',#8830);
#798=PLANE('',#8831);
#799=PLANE('',#8832);
#800=PLANE('',#8833);
#801=PLANE('',#8835);
#802=PLANE('',#8836);
#803=PLANE('',#8837);
#804=PLANE('',#8838);
#805=PLANE('',#8839);
#806=PLANE('',#8840);
#807=PLANE('',#8848);
#808=PLANE('',#8852);
#809=PLANE('',#8856);
#810=PLANE('',#8860);
#811=PLANE('',#8888);
#812=PLANE('',#8898);
#813=PLANE('',#8900);
#814=PLANE('',#8901);
#815=PLANE('',#8902);
#816=PLANE('',#8903);
#817=PLANE('',#8904);
#818=PLANE('',#8905);
#819=PLANE('',#8906);
#820=PLANE('',#8909);
#821=PLANE('',#8910);
#822=PLANE('',#8911);
#823=PLANE('',#8912);
#824=PLANE('',#8913);
#825=PLANE('',#8914);
#826=PLANE('',#8915);
#827=PLANE('',#8932);
#828=PLANE('',#8939);
#829=PLANE('',#8940);
#830=PLANE('',#8957);
#831=PLANE('',#8964);
#832=PLANE('',#8965);
#833=PLANE('',#8970);
#834=PLANE('',#8975);
#835=PLANE('',#8980);
#836=PLANE('',#8985);
#837=PLANE('',#8998);
#838=PLANE('',#9005);
#839=PLANE('',#9006);
#840=PLANE('',#9008);
#841=PLANE('',#9009);
#842=PLANE('',#9010);
#843=PLANE('',#9011);
#844=PLANE('',#9012);
#845=PLANE('',#9013);
#846=PLANE('',#9018);
#847=PLANE('',#9022);
#848=PLANE('',#9023);
#849=PLANE('',#9024);
#850=PLANE('',#9025);
#851=PLANE('',#9026);
#852=PLANE('',#9027);
#853=PLANE('',#9028);
#854=PLANE('',#9033);
#855=PLANE('',#9037);
#856=PLANE('',#9038);
#857=PLANE('',#9039);
#858=PLANE('',#9040);
#859=PLANE('',#9041);
#860=PLANE('',#9042);
#861=PLANE('',#9043);
#862=PLANE('',#9048);
#863=PLANE('',#9049);
#864=PLANE('',#9054);
#865=PLANE('',#9057);
#866=PLANE('',#9059);
#867=PLANE('',#9060);
#868=PLANE('',#9061);
#869=PLANE('',#9062);
#870=PLANE('',#9063);
#871=PLANE('',#9064);
#872=PLANE('',#9065);
#873=PLANE('',#9066);
#874=PLANE('',#9067);
#875=PLANE('',#9068);
#876=PLANE('',#9069);
#877=PLANE('',#9070);
#878=PLANE('',#9071);
#879=PLANE('',#9072);
#880=PLANE('',#9073);
#881=PLANE('',#9074);
#882=PLANE('',#9075);
#883=PLANE('',#9076);
#884=PLANE('',#9077);
#885=PLANE('',#9078);
#886=PLANE('',#9079);
#887=PLANE('',#9080);
#888=PLANE('',#9081);
#889=PLANE('',#9082);
#890=PLANE('',#9083);
#891=PLANE('',#9084);
#892=PLANE('',#9085);
#893=PLANE('',#9086);
#894=PLANE('',#9087);
#895=PLANE('',#9088);
#896=PLANE('',#9089);
#897=PLANE('',#9090);
#898=PLANE('',#9091);
#899=PLANE('',#9092);
#900=PLANE('',#9093);
#901=PLANE('',#9094);
#902=PLANE('',#9098);
#903=PLANE('',#9099);
#904=PLANE('',#9100);
#905=PLANE('',#9101);
#906=PLANE('',#9102);
#907=PLANE('',#9103);
#908=PLANE('',#9104);
#909=PLANE('',#9105);
#910=PLANE('',#9106);
#911=PLANE('',#9107);
#912=PLANE('',#9109);
#913=PLANE('',#9110);
#914=PLANE('',#9111);
#915=PLANE('',#9113);
#916=PLANE('',#9114);
#917=PLANE('',#9115);
#918=PLANE('',#9116);
#919=PLANE('',#9117);
#920=PLANE('',#9118);
#921=PLANE('',#9125);
#922=PLANE('',#9126);
#923=PLANE('',#9127);
#924=PLANE('',#9128);
#925=PLANE('',#9135);
#926=PLANE('',#9139);
#927=PLANE('',#9141);
#928=PLANE('',#9142);
#929=PLANE('',#9143);
#930=PLANE('',#9144);
#931=PLANE('',#9145);
#932=PLANE('',#9146);
#933=PLANE('',#9147);
#934=PLANE('',#9148);
#935=PLANE('',#9149);
#936=PLANE('',#9151);
#937=PLANE('',#9159);
#938=PLANE('',#9179);
#939=PLANE('',#9182);
#940=PLANE('',#9194);
#941=PLANE('',#9203);
#942=PLANE('',#9236);
#943=PLANE('',#9241);
#944=PLANE('',#9246);
#945=PLANE('',#9251);
#946=PLANE('',#9256);
#947=PLANE('',#9261);
#948=PLANE('',#9270);
#949=PLANE('',#9274);
#950=PLANE('',#9275);
#951=PLANE('',#9277);
#952=PLANE('',#9282);
#953=PLANE('',#9285);
#954=PLANE('',#9290);
#955=PLANE('',#9300);
#956=PLANE('',#9302);
#957=PLANE('',#9303);
#958=PLANE('',#9305);
#959=PLANE('',#9306);
#960=PLANE('',#9307);
#961=PLANE('',#9312);
#962=PLANE('',#9316);
#963=PLANE('',#9320);
#964=PLANE('',#9324);
#965=PLANE('',#9328);
#966=PLANE('',#9332);
#967=PLANE('',#9335);
#968=PLANE('',#9336);
#969=PLANE('',#9339);
#970=PLANE('',#9340);
#971=PLANE('',#9345);
#972=PLANE('',#9351);
#973=PLANE('',#9352);
#974=PLANE('',#9353);
#975=PLANE('',#9354);
#976=PLANE('',#9355);
#977=PLANE('',#9356);
#978=PLANE('',#9357);
#979=PLANE('',#9358);
#980=PLANE('',#9359);
#981=PLANE('',#9364);
#982=PLANE('',#9365);
#983=PLANE('',#9373);
#984=PLANE('',#9388);
#985=PLANE('',#9394);
#986=PLANE('',#9395);
#987=PLANE('',#9397);
#988=PLANE('',#9400);
#989=PLANE('',#9401);
#990=PLANE('',#9403);
#991=PLANE('',#9404);
#992=PLANE('',#9408);
#993=PLANE('',#9416);
#994=PLANE('',#9417);
#995=PLANE('',#9425);
#996=PLANE('',#9426);
#997=PLANE('',#9428);
#998=PLANE('',#9433);
#999=PLANE('',#9440);
#1000=PLANE('',#9441);
#1001=PLANE('',#9446);
#1002=PLANE('',#9450);
#1003=PLANE('',#9451);
#1004=PLANE('',#9454);
#1005=PLANE('',#9462);
#1006=PLANE('',#9463);
#1007=PLANE('',#9471);
#1008=PLANE('',#9472);
#1009=PLANE('',#9480);
#1010=PLANE('',#9481);
#1011=PLANE('',#9489);
#1012=PLANE('',#9490);
#1013=PLANE('',#9498);
#1014=PLANE('',#9499);
#1015=PLANE('',#9501);
#1016=PLANE('',#9503);
#1017=PLANE('',#9504);
#1018=PLANE('',#9505);
#1019=PLANE('',#9506);
#1020=PLANE('',#9507);
#1021=PLANE('',#9508);
#1022=PLANE('',#9509);
#1023=PLANE('',#9510);
#1024=PLANE('',#9516);
#1025=PLANE('',#9517);
#1026=PLANE('',#9518);
#1027=PLANE('',#9519);
#1028=PLANE('',#9520);
#1029=PLANE('',#9521);
#1030=PLANE('',#9522);
#1031=PLANE('',#9523);
#1032=PLANE('',#9524);
#1033=PLANE('',#9526);
#1034=PLANE('',#9534);
#1035=PLANE('',#9540);
#1036=PLANE('',#9548);
#1037=PLANE('',#9556);
#1038=PLANE('',#9557);
#1039=PLANE('',#9558);
#1040=PLANE('',#9559);
#1041=PLANE('',#9560);
#1042=PLANE('',#9561);
#1043=PLANE('',#9562);
#1044=PLANE('',#9563);
#1045=PLANE('',#9564);
#1046=PLANE('',#9644);
#1047=PLANE('',#9645);
#1048=PLANE('',#9647);
#1049=PLANE('',#9650);
#1050=PLANE('',#9658);
#1051=PLANE('',#9659);
#1052=PLANE('',#9667);
#1053=PLANE('',#9668);
#1054=PLANE('',#9677);
#1055=PLANE('',#9678);
#1056=PLANE('',#9679);
#1057=PLANE('',#9680);
#1058=PLANE('',#9682);
#1059=PLANE('',#9683);
#1060=PLANE('',#9684);
#1061=PLANE('',#9685);
#1062=PLANE('',#9690);
#1063=PLANE('',#9695);
#1064=PLANE('',#9696);
#1065=PLANE('',#9697);
#1066=PLANE('',#9703);
#1067=PLANE('',#9707);
#1068=PLANE('',#9708);
#1069=PLANE('',#9709);
#1070=PLANE('',#9710);
#1071=PLANE('',#9711);
#1072=PLANE('',#9712);
#1073=PLANE('',#9714);
#1074=PLANE('',#9719);
#1075=PLANE('',#9722);
#1076=PLANE('',#9727);
#1077=PLANE('',#9728);
#1078=PLANE('',#9730);
#1079=PLANE('',#9731);
#1080=PLANE('',#9732);
#1081=PLANE('',#9733);
#1082=PLANE('',#9734);
#1083=PLANE('',#9735);
#1084=PLANE('',#9736);
#1085=PLANE('',#9737);
#1086=PLANE('',#9745);
#1087=FACE_OUTER_BOUND('',#1573,.T.);
#1088=FACE_OUTER_BOUND('',#1574,.T.);
#1089=FACE_OUTER_BOUND('',#1575,.T.);
#1090=FACE_OUTER_BOUND('',#1576,.T.);
#1091=FACE_OUTER_BOUND('',#1577,.T.);
#1092=FACE_OUTER_BOUND('',#1578,.T.);
#1093=FACE_OUTER_BOUND('',#1579,.T.);
#1094=FACE_OUTER_BOUND('',#1580,.T.);
#1095=FACE_OUTER_BOUND('',#1581,.T.);
#1096=FACE_OUTER_BOUND('',#1582,.T.);
#1097=FACE_OUTER_BOUND('',#1583,.T.);
#1098=FACE_OUTER_BOUND('',#1584,.T.);
#1099=FACE_OUTER_BOUND('',#1585,.T.);
#1100=FACE_OUTER_BOUND('',#1586,.T.);
#1101=FACE_OUTER_BOUND('',#1587,.T.);
#1102=FACE_OUTER_BOUND('',#1588,.T.);
#1103=FACE_OUTER_BOUND('',#1589,.T.);
#1104=FACE_OUTER_BOUND('',#1602,.T.);
#1105=FACE_OUTER_BOUND('',#1615,.T.);
#1106=FACE_OUTER_BOUND('',#1616,.T.);
#1107=FACE_OUTER_BOUND('',#1617,.T.);
#1108=FACE_OUTER_BOUND('',#1618,.T.);
#1109=FACE_OUTER_BOUND('',#1619,.T.);
#1110=FACE_OUTER_BOUND('',#1620,.T.);
#1111=FACE_OUTER_BOUND('',#1621,.T.);
#1112=FACE_OUTER_BOUND('',#1622,.T.);
#1113=FACE_OUTER_BOUND('',#1623,.T.);
#1114=FACE_OUTER_BOUND('',#1628,.T.);
#1115=FACE_OUTER_BOUND('',#1633,.T.);
#1116=FACE_OUTER_BOUND('',#1634,.T.);
#1117=FACE_OUTER_BOUND('',#1635,.T.);
#1118=FACE_OUTER_BOUND('',#1636,.T.);
#1119=FACE_OUTER_BOUND('',#1637,.T.);
#1120=FACE_OUTER_BOUND('',#1638,.T.);
#1121=FACE_OUTER_BOUND('',#1639,.T.);
#1122=FACE_OUTER_BOUND('',#1640,.T.);
#1123=FACE_OUTER_BOUND('',#1641,.T.);
#1124=FACE_OUTER_BOUND('',#1642,.T.);
#1125=FACE_OUTER_BOUND('',#1643,.T.);
#1126=FACE_OUTER_BOUND('',#1644,.T.);
#1127=FACE_OUTER_BOUND('',#1645,.T.);
#1128=FACE_OUTER_BOUND('',#1646,.T.);
#1129=FACE_OUTER_BOUND('',#1647,.T.);
#1130=FACE_OUTER_BOUND('',#1648,.T.);
#1131=FACE_OUTER_BOUND('',#1649,.T.);
#1132=FACE_OUTER_BOUND('',#1650,.T.);
#1133=FACE_OUTER_BOUND('',#1651,.T.);
#1134=FACE_OUTER_BOUND('',#1652,.T.);
#1135=FACE_OUTER_BOUND('',#1653,.T.);
#1136=FACE_OUTER_BOUND('',#1654,.T.);
#1137=FACE_OUTER_BOUND('',#1655,.T.);
#1138=FACE_OUTER_BOUND('',#1656,.T.);
#1139=FACE_OUTER_BOUND('',#1657,.T.);
#1140=FACE_OUTER_BOUND('',#1658,.T.);
#1141=FACE_OUTER_BOUND('',#1659,.T.);
#1142=FACE_OUTER_BOUND('',#1660,.T.);
#1143=FACE_OUTER_BOUND('',#1661,.T.);
#1144=FACE_OUTER_BOUND('',#1662,.T.);
#1145=FACE_OUTER_BOUND('',#1663,.T.);
#1146=FACE_OUTER_BOUND('',#1665,.T.);
#1147=FACE_OUTER_BOUND('',#1666,.T.);
#1148=FACE_OUTER_BOUND('',#1667,.T.);
#1149=FACE_OUTER_BOUND('',#1668,.T.);
#1150=FACE_OUTER_BOUND('',#1675,.T.);
#1151=FACE_OUTER_BOUND('',#1681,.T.);
#1152=FACE_OUTER_BOUND('',#1687,.T.);
#1153=FACE_OUTER_BOUND('',#1688,.T.);
#1154=FACE_OUTER_BOUND('',#1689,.T.);
#1155=FACE_OUTER_BOUND('',#1690,.T.);
#1156=FACE_OUTER_BOUND('',#1691,.T.);
#1157=FACE_OUTER_BOUND('',#1692,.T.);
#1158=FACE_OUTER_BOUND('',#1693,.T.);
#1159=FACE_OUTER_BOUND('',#1700,.T.);
#1160=FACE_OUTER_BOUND('',#1701,.T.);
#1161=FACE_OUTER_BOUND('',#1703,.T.);
#1162=FACE_OUTER_BOUND('',#1704,.T.);
#1163=FACE_OUTER_BOUND('',#1705,.T.);
#1164=FACE_OUTER_BOUND('',#1706,.T.);
#1165=FACE_OUTER_BOUND('',#1711,.T.);
#1166=FACE_OUTER_BOUND('',#1712,.T.);
#1167=FACE_OUTER_BOUND('',#1713,.T.);
#1168=FACE_OUTER_BOUND('',#1714,.T.);
#1169=FACE_OUTER_BOUND('',#1715,.T.);
#1170=FACE_OUTER_BOUND('',#1716,.T.);
#1171=FACE_OUTER_BOUND('',#1718,.T.);
#1172=FACE_OUTER_BOUND('',#1719,.T.);
#1173=FACE_OUTER_BOUND('',#1720,.T.);
#1174=FACE_OUTER_BOUND('',#1726,.T.);
#1175=FACE_OUTER_BOUND('',#1732,.T.);
#1176=FACE_OUTER_BOUND('',#1733,.T.);
#1177=FACE_OUTER_BOUND('',#1734,.T.);
#1178=FACE_OUTER_BOUND('',#1735,.T.);
#1179=FACE_OUTER_BOUND('',#1736,.T.);
#1180=FACE_OUTER_BOUND('',#1737,.T.);
#1181=FACE_OUTER_BOUND('',#1739,.T.);
#1182=FACE_OUTER_BOUND('',#1740,.T.);
#1183=FACE_OUTER_BOUND('',#1741,.T.);
#1184=FACE_OUTER_BOUND('',#1747,.T.);
#1185=FACE_OUTER_BOUND('',#1753,.T.);
#1186=FACE_OUTER_BOUND('',#1754,.T.);
#1187=FACE_OUTER_BOUND('',#1756,.T.);
#1188=FACE_OUTER_BOUND('',#1757,.T.);
#1189=FACE_OUTER_BOUND('',#1759,.T.);
#1190=FACE_OUTER_BOUND('',#1760,.T.);
#1191=FACE_OUTER_BOUND('',#1762,.T.);
#1192=FACE_OUTER_BOUND('',#1763,.T.);
#1193=FACE_OUTER_BOUND('',#1765,.T.);
#1194=FACE_OUTER_BOUND('',#1766,.T.);
#1195=FACE_OUTER_BOUND('',#1767,.T.);
#1196=FACE_OUTER_BOUND('',#1768,.T.);
#1197=FACE_OUTER_BOUND('',#1769,.T.);
#1198=FACE_OUTER_BOUND('',#1770,.T.);
#1199=FACE_OUTER_BOUND('',#1772,.T.);
#1200=FACE_OUTER_BOUND('',#1773,.T.);
#1201=FACE_OUTER_BOUND('',#1774,.T.);
#1202=FACE_OUTER_BOUND('',#1780,.T.);
#1203=FACE_OUTER_BOUND('',#1786,.T.);
#1204=FACE_OUTER_BOUND('',#1787,.T.);
#1205=FACE_OUTER_BOUND('',#1788,.T.);
#1206=FACE_OUTER_BOUND('',#1789,.T.);
#1207=FACE_OUTER_BOUND('',#1790,.T.);
#1208=FACE_OUTER_BOUND('',#1791,.T.);
#1209=FACE_OUTER_BOUND('',#1792,.T.);
#1210=FACE_OUTER_BOUND('',#1793,.T.);
#1211=FACE_OUTER_BOUND('',#1794,.T.);
#1212=FACE_OUTER_BOUND('',#1795,.T.);
#1213=FACE_OUTER_BOUND('',#1796,.T.);
#1214=FACE_OUTER_BOUND('',#1797,.T.);
#1215=FACE_OUTER_BOUND('',#1798,.T.);
#1216=FACE_OUTER_BOUND('',#1799,.T.);
#1217=FACE_OUTER_BOUND('',#1800,.T.);
#1218=FACE_OUTER_BOUND('',#1801,.T.);
#1219=FACE_OUTER_BOUND('',#1804,.T.);
#1220=FACE_OUTER_BOUND('',#1805,.T.);
#1221=FACE_OUTER_BOUND('',#1806,.T.);
#1222=FACE_OUTER_BOUND('',#1807,.T.);
#1223=FACE_OUTER_BOUND('',#1808,.T.);
#1224=FACE_OUTER_BOUND('',#1809,.T.);
#1225=FACE_OUTER_BOUND('',#1810,.T.);
#1226=FACE_OUTER_BOUND('',#1811,.T.);
#1227=FACE_OUTER_BOUND('',#1812,.T.);
#1228=FACE_OUTER_BOUND('',#1813,.T.);
#1229=FACE_OUTER_BOUND('',#1816,.T.);
#1230=FACE_OUTER_BOUND('',#1817,.T.);
#1231=FACE_OUTER_BOUND('',#1818,.T.);
#1232=FACE_OUTER_BOUND('',#1820,.T.);
#1233=FACE_OUTER_BOUND('',#1821,.T.);
#1234=FACE_OUTER_BOUND('',#1823,.T.);
#1235=FACE_OUTER_BOUND('',#1824,.T.);
#1236=FACE_OUTER_BOUND('',#1825,.T.);
#1237=FACE_OUTER_BOUND('',#1826,.T.);
#1238=FACE_OUTER_BOUND('',#1827,.T.);
#1239=FACE_OUTER_BOUND('',#1828,.T.);
#1240=FACE_OUTER_BOUND('',#1829,.T.);
#1241=FACE_OUTER_BOUND('',#1830,.T.);
#1242=FACE_OUTER_BOUND('',#1831,.T.);
#1243=FACE_OUTER_BOUND('',#1832,.T.);
#1244=FACE_OUTER_BOUND('',#1833,.T.);
#1245=FACE_OUTER_BOUND('',#1834,.T.);
#1246=FACE_OUTER_BOUND('',#1835,.T.);
#1247=FACE_OUTER_BOUND('',#1836,.T.);
#1248=FACE_OUTER_BOUND('',#1837,.T.);
#1249=FACE_OUTER_BOUND('',#1838,.T.);
#1250=FACE_OUTER_BOUND('',#1839,.T.);
#1251=FACE_OUTER_BOUND('',#1840,.T.);
#1252=FACE_OUTER_BOUND('',#1841,.T.);
#1253=FACE_OUTER_BOUND('',#1842,.T.);
#1254=FACE_OUTER_BOUND('',#1843,.T.);
#1255=FACE_OUTER_BOUND('',#1844,.T.);
#1256=FACE_OUTER_BOUND('',#1845,.T.);
#1257=FACE_OUTER_BOUND('',#1846,.T.);
#1258=FACE_OUTER_BOUND('',#1847,.T.);
#1259=FACE_OUTER_BOUND('',#1848,.T.);
#1260=FACE_OUTER_BOUND('',#1849,.T.);
#1261=FACE_OUTER_BOUND('',#1850,.T.);
#1262=FACE_OUTER_BOUND('',#1851,.T.);
#1263=FACE_OUTER_BOUND('',#1852,.T.);
#1264=FACE_OUTER_BOUND('',#1853,.T.);
#1265=FACE_OUTER_BOUND('',#1854,.T.);
#1266=FACE_OUTER_BOUND('',#1855,.T.);
#1267=FACE_OUTER_BOUND('',#1856,.T.);
#1268=FACE_OUTER_BOUND('',#1857,.T.);
#1269=FACE_OUTER_BOUND('',#1858,.T.);
#1270=FACE_OUTER_BOUND('',#1859,.T.);
#1271=FACE_OUTER_BOUND('',#1860,.T.);
#1272=FACE_OUTER_BOUND('',#1861,.T.);
#1273=FACE_OUTER_BOUND('',#1862,.T.);
#1274=FACE_OUTER_BOUND('',#1863,.T.);
#1275=FACE_OUTER_BOUND('',#1864,.T.);
#1276=FACE_OUTER_BOUND('',#1865,.T.);
#1277=FACE_OUTER_BOUND('',#1866,.T.);
#1278=FACE_OUTER_BOUND('',#1867,.T.);
#1279=FACE_OUTER_BOUND('',#1868,.T.);
#1280=FACE_OUTER_BOUND('',#1869,.T.);
#1281=FACE_OUTER_BOUND('',#1870,.T.);
#1282=FACE_OUTER_BOUND('',#1872,.T.);
#1283=FACE_OUTER_BOUND('',#1874,.T.);
#1284=FACE_OUTER_BOUND('',#1875,.T.);
#1285=FACE_OUTER_BOUND('',#1876,.T.);
#1286=FACE_OUTER_BOUND('',#1878,.T.);
#1287=FACE_OUTER_BOUND('',#1879,.T.);
#1288=FACE_OUTER_BOUND('',#1880,.T.);
#1289=FACE_OUTER_BOUND('',#1881,.T.);
#1290=FACE_OUTER_BOUND('',#1882,.T.);
#1291=FACE_OUTER_BOUND('',#1883,.T.);
#1292=FACE_OUTER_BOUND('',#1884,.T.);
#1293=FACE_OUTER_BOUND('',#1885,.T.);
#1294=FACE_OUTER_BOUND('',#1886,.T.);
#1295=FACE_OUTER_BOUND('',#1887,.T.);
#1296=FACE_OUTER_BOUND('',#1888,.T.);
#1297=FACE_OUTER_BOUND('',#1889,.T.);
#1298=FACE_OUTER_BOUND('',#1890,.T.);
#1299=FACE_OUTER_BOUND('',#1891,.T.);
#1300=FACE_OUTER_BOUND('',#1893,.T.);
#1301=FACE_OUTER_BOUND('',#1894,.T.);
#1302=FACE_OUTER_BOUND('',#1896,.T.);
#1303=FACE_OUTER_BOUND('',#1897,.T.);
#1304=FACE_OUTER_BOUND('',#1898,.T.);
#1305=FACE_OUTER_BOUND('',#1899,.T.);
#1306=FACE_OUTER_BOUND('',#1900,.T.);
#1307=FACE_OUTER_BOUND('',#1901,.T.);
#1308=FACE_OUTER_BOUND('',#1902,.T.);
#1309=FACE_OUTER_BOUND('',#1903,.T.);
#1310=FACE_OUTER_BOUND('',#1904,.T.);
#1311=FACE_OUTER_BOUND('',#1905,.T.);
#1312=FACE_OUTER_BOUND('',#1906,.T.);
#1313=FACE_OUTER_BOUND('',#1907,.T.);
#1314=FACE_OUTER_BOUND('',#1908,.T.);
#1315=FACE_OUTER_BOUND('',#1909,.T.);
#1316=FACE_OUTER_BOUND('',#1911,.T.);
#1317=FACE_OUTER_BOUND('',#1912,.T.);
#1318=FACE_OUTER_BOUND('',#1913,.T.);
#1319=FACE_OUTER_BOUND('',#1914,.T.);
#1320=FACE_OUTER_BOUND('',#1915,.T.);
#1321=FACE_OUTER_BOUND('',#1916,.T.);
#1322=FACE_OUTER_BOUND('',#1917,.T.);
#1323=FACE_OUTER_BOUND('',#1919,.T.);
#1324=FACE_OUTER_BOUND('',#1920,.T.);
#1325=FACE_OUTER_BOUND('',#1922,.T.);
#1326=FACE_OUTER_BOUND('',#1923,.T.);
#1327=FACE_OUTER_BOUND('',#1924,.T.);
#1328=FACE_OUTER_BOUND('',#1925,.T.);
#1329=FACE_OUTER_BOUND('',#1927,.T.);
#1330=FACE_OUTER_BOUND('',#1928,.T.);
#1331=FACE_OUTER_BOUND('',#1929,.T.);
#1332=FACE_OUTER_BOUND('',#1930,.T.);
#1333=FACE_OUTER_BOUND('',#1932,.T.);
#1334=FACE_OUTER_BOUND('',#1933,.T.);
#1335=FACE_OUTER_BOUND('',#1934,.T.);
#1336=FACE_OUTER_BOUND('',#1935,.T.);
#1337=FACE_OUTER_BOUND('',#1936,.T.);
#1338=FACE_OUTER_BOUND('',#1937,.T.);
#1339=FACE_OUTER_BOUND('',#1938,.T.);
#1340=FACE_OUTER_BOUND('',#1939,.T.);
#1341=FACE_OUTER_BOUND('',#1940,.T.);
#1342=FACE_OUTER_BOUND('',#1941,.T.);
#1343=FACE_OUTER_BOUND('',#1942,.T.);
#1344=FACE_OUTER_BOUND('',#1943,.T.);
#1345=FACE_OUTER_BOUND('',#1944,.T.);
#1346=FACE_OUTER_BOUND('',#1945,.T.);
#1347=FACE_OUTER_BOUND('',#1946,.T.);
#1348=FACE_OUTER_BOUND('',#1947,.T.);
#1349=FACE_OUTER_BOUND('',#1948,.T.);
#1350=FACE_OUTER_BOUND('',#1949,.T.);
#1351=FACE_OUTER_BOUND('',#1950,.T.);
#1352=FACE_OUTER_BOUND('',#1951,.T.);
#1353=FACE_OUTER_BOUND('',#1952,.T.);
#1354=FACE_OUTER_BOUND('',#1953,.T.);
#1355=FACE_OUTER_BOUND('',#1954,.T.);
#1356=FACE_OUTER_BOUND('',#1955,.T.);
#1357=FACE_OUTER_BOUND('',#1956,.T.);
#1358=FACE_OUTER_BOUND('',#1957,.T.);
#1359=FACE_OUTER_BOUND('',#1958,.T.);
#1360=FACE_OUTER_BOUND('',#1960,.T.);
#1361=FACE_OUTER_BOUND('',#1961,.T.);
#1362=FACE_OUTER_BOUND('',#1963,.T.);
#1363=FACE_OUTER_BOUND('',#1964,.T.);
#1364=FACE_OUTER_BOUND('',#1966,.T.);
#1365=FACE_OUTER_BOUND('',#1967,.T.);
#1366=FACE_OUTER_BOUND('',#1969,.T.);
#1367=FACE_OUTER_BOUND('',#1970,.T.);
#1368=FACE_OUTER_BOUND('',#1972,.T.);
#1369=FACE_OUTER_BOUND('',#1973,.T.);
#1370=FACE_OUTER_BOUND('',#1974,.T.);
#1371=FACE_OUTER_BOUND('',#1975,.T.);
#1372=FACE_OUTER_BOUND('',#1976,.T.);
#1373=FACE_OUTER_BOUND('',#1977,.T.);
#1374=FACE_OUTER_BOUND('',#1978,.T.);
#1375=FACE_OUTER_BOUND('',#1980,.T.);
#1376=FACE_OUTER_BOUND('',#1981,.T.);
#1377=FACE_OUTER_BOUND('',#1983,.T.);
#1378=FACE_OUTER_BOUND('',#1984,.T.);
#1379=FACE_OUTER_BOUND('',#1986,.T.);
#1380=FACE_OUTER_BOUND('',#1987,.T.);
#1381=FACE_OUTER_BOUND('',#1989,.T.);
#1382=FACE_OUTER_BOUND('',#1990,.T.);
#1383=FACE_OUTER_BOUND('',#1992,.T.);
#1384=FACE_OUTER_BOUND('',#1993,.T.);
#1385=FACE_OUTER_BOUND('',#1995,.T.);
#1386=FACE_OUTER_BOUND('',#1997,.T.);
#1387=FACE_OUTER_BOUND('',#1998,.T.);
#1388=FACE_OUTER_BOUND('',#1999,.T.);
#1389=FACE_OUTER_BOUND('',#2000,.T.);
#1390=FACE_OUTER_BOUND('',#2001,.T.);
#1391=FACE_OUTER_BOUND('',#2003,.T.);
#1392=FACE_OUTER_BOUND('',#2005,.T.);
#1393=FACE_OUTER_BOUND('',#2007,.T.);
#1394=FACE_OUTER_BOUND('',#2009,.T.);
#1395=FACE_OUTER_BOUND('',#2010,.T.);
#1396=FACE_OUTER_BOUND('',#2011,.T.);
#1397=FACE_OUTER_BOUND('',#2012,.T.);
#1398=FACE_OUTER_BOUND('',#2013,.T.);
#1399=FACE_OUTER_BOUND('',#2014,.T.);
#1400=FACE_OUTER_BOUND('',#2015,.T.);
#1401=FACE_OUTER_BOUND('',#2016,.T.);
#1402=FACE_OUTER_BOUND('',#2017,.T.);
#1403=FACE_OUTER_BOUND('',#2019,.T.);
#1404=FACE_OUTER_BOUND('',#2020,.T.);
#1405=FACE_OUTER_BOUND('',#2021,.T.);
#1406=FACE_OUTER_BOUND('',#2022,.T.);
#1407=FACE_OUTER_BOUND('',#2023,.T.);
#1408=FACE_OUTER_BOUND('',#2024,.T.);
#1409=FACE_OUTER_BOUND('',#2025,.T.);
#1410=FACE_OUTER_BOUND('',#2027,.T.);
#1411=FACE_OUTER_BOUND('',#2028,.T.);
#1412=FACE_OUTER_BOUND('',#2029,.T.);
#1413=FACE_OUTER_BOUND('',#2030,.T.);
#1414=FACE_OUTER_BOUND('',#2031,.T.);
#1415=FACE_OUTER_BOUND('',#2032,.T.);
#1416=FACE_OUTER_BOUND('',#2035,.T.);
#1417=FACE_OUTER_BOUND('',#2036,.T.);
#1418=FACE_OUTER_BOUND('',#2037,.T.);
#1419=FACE_OUTER_BOUND('',#2038,.T.);
#1420=FACE_OUTER_BOUND('',#2039,.T.);
#1421=FACE_OUTER_BOUND('',#2040,.T.);
#1422=FACE_OUTER_BOUND('',#2042,.T.);
#1423=FACE_OUTER_BOUND('',#2043,.T.);
#1424=FACE_OUTER_BOUND('',#2045,.T.);
#1425=FACE_OUTER_BOUND('',#2046,.T.);
#1426=FACE_OUTER_BOUND('',#2048,.T.);
#1427=FACE_OUTER_BOUND('',#2049,.T.);
#1428=FACE_OUTER_BOUND('',#2050,.T.);
#1429=FACE_OUTER_BOUND('',#2051,.T.);
#1430=FACE_OUTER_BOUND('',#2052,.T.);
#1431=FACE_OUTER_BOUND('',#2053,.T.);
#1432=FACE_OUTER_BOUND('',#2054,.T.);
#1433=FACE_OUTER_BOUND('',#2055,.T.);
#1434=FACE_OUTER_BOUND('',#2057,.T.);
#1435=FACE_OUTER_BOUND('',#2059,.T.);
#1436=FACE_OUTER_BOUND('',#2060,.T.);
#1437=FACE_OUTER_BOUND('',#2061,.T.);
#1438=FACE_OUTER_BOUND('',#2062,.T.);
#1439=FACE_OUTER_BOUND('',#2064,.T.);
#1440=FACE_OUTER_BOUND('',#2066,.T.);
#1441=FACE_OUTER_BOUND('',#2068,.T.);
#1442=FACE_OUTER_BOUND('',#2070,.T.);
#1443=FACE_OUTER_BOUND('',#2071,.T.);
#1444=FACE_OUTER_BOUND('',#2072,.T.);
#1445=FACE_OUTER_BOUND('',#2073,.T.);
#1446=FACE_OUTER_BOUND('',#2074,.T.);
#1447=FACE_OUTER_BOUND('',#2076,.T.);
#1448=FACE_OUTER_BOUND('',#2078,.T.);
#1449=FACE_OUTER_BOUND('',#2079,.T.);
#1450=FACE_OUTER_BOUND('',#2080,.T.);
#1451=FACE_OUTER_BOUND('',#2081,.T.);
#1452=FACE_OUTER_BOUND('',#2083,.T.);
#1453=FACE_OUTER_BOUND('',#2085,.T.);
#1454=FACE_OUTER_BOUND('',#2086,.T.);
#1455=FACE_OUTER_BOUND('',#2087,.T.);
#1456=FACE_OUTER_BOUND('',#2089,.T.);
#1457=FACE_OUTER_BOUND('',#2091,.T.);
#1458=FACE_OUTER_BOUND('',#2092,.T.);
#1459=FACE_OUTER_BOUND('',#2093,.T.);
#1460=FACE_OUTER_BOUND('',#2095,.T.);
#1461=FACE_OUTER_BOUND('',#2097,.T.);
#1462=FACE_OUTER_BOUND('',#2098,.T.);
#1463=FACE_OUTER_BOUND('',#2099,.T.);
#1464=FACE_OUTER_BOUND('',#2101,.T.);
#1465=FACE_OUTER_BOUND('',#2103,.T.);
#1466=FACE_OUTER_BOUND('',#2104,.T.);
#1467=FACE_OUTER_BOUND('',#2105,.T.);
#1468=FACE_OUTER_BOUND('',#2107,.T.);
#1469=FACE_OUTER_BOUND('',#2109,.T.);
#1470=FACE_OUTER_BOUND('',#2110,.T.);
#1471=FACE_OUTER_BOUND('',#2111,.T.);
#1472=FACE_OUTER_BOUND('',#2112,.T.);
#1473=FACE_OUTER_BOUND('',#2113,.T.);
#1474=FACE_OUTER_BOUND('',#2114,.T.);
#1475=FACE_OUTER_BOUND('',#2115,.T.);
#1476=FACE_OUTER_BOUND('',#2116,.T.);
#1477=FACE_OUTER_BOUND('',#2117,.T.);
#1478=FACE_OUTER_BOUND('',#2119,.T.);
#1479=FACE_OUTER_BOUND('',#2120,.T.);
#1480=FACE_OUTER_BOUND('',#2121,.T.);
#1481=FACE_OUTER_BOUND('',#2122,.T.);
#1482=FACE_OUTER_BOUND('',#2123,.T.);
#1483=FACE_OUTER_BOUND('',#2124,.T.);
#1484=FACE_OUTER_BOUND('',#2125,.T.);
#1485=FACE_OUTER_BOUND('',#2126,.T.);
#1486=FACE_OUTER_BOUND('',#2127,.T.);
#1487=FACE_OUTER_BOUND('',#2128,.T.);
#1488=FACE_OUTER_BOUND('',#2129,.T.);
#1489=FACE_OUTER_BOUND('',#2130,.T.);
#1490=FACE_OUTER_BOUND('',#2131,.T.);
#1491=FACE_OUTER_BOUND('',#2132,.T.);
#1492=FACE_OUTER_BOUND('',#2133,.T.);
#1493=FACE_OUTER_BOUND('',#2134,.T.);
#1494=FACE_OUTER_BOUND('',#2136,.T.);
#1495=FACE_OUTER_BOUND('',#2137,.T.);
#1496=FACE_OUTER_BOUND('',#2138,.T.);
#1497=FACE_OUTER_BOUND('',#2139,.T.);
#1498=FACE_OUTER_BOUND('',#2140,.T.);
#1499=FACE_OUTER_BOUND('',#2141,.T.);
#1500=FACE_OUTER_BOUND('',#2142,.T.);
#1501=FACE_OUTER_BOUND('',#2144,.T.);
#1502=FACE_OUTER_BOUND('',#2145,.T.);
#1503=FACE_OUTER_BOUND('',#2146,.T.);
#1504=FACE_OUTER_BOUND('',#2147,.T.);
#1505=FACE_OUTER_BOUND('',#2148,.T.);
#1506=FACE_OUTER_BOUND('',#2149,.T.);
#1507=FACE_OUTER_BOUND('',#2150,.T.);
#1508=FACE_OUTER_BOUND('',#2151,.T.);
#1509=FACE_OUTER_BOUND('',#2152,.T.);
#1510=FACE_OUTER_BOUND('',#2153,.T.);
#1511=FACE_OUTER_BOUND('',#2154,.T.);
#1512=FACE_OUTER_BOUND('',#2155,.T.);
#1513=FACE_OUTER_BOUND('',#2156,.T.);
#1514=FACE_OUTER_BOUND('',#2157,.T.);
#1515=FACE_OUTER_BOUND('',#2158,.T.);
#1516=FACE_OUTER_BOUND('',#2159,.T.);
#1517=FACE_OUTER_BOUND('',#2160,.T.);
#1518=FACE_OUTER_BOUND('',#2163,.T.);
#1519=FACE_OUTER_BOUND('',#2164,.T.);
#1520=FACE_OUTER_BOUND('',#2165,.T.);
#1521=FACE_OUTER_BOUND('',#2168,.T.);
#1522=FACE_OUTER_BOUND('',#2169,.T.);
#1523=FACE_OUTER_BOUND('',#2170,.T.);
#1524=FACE_OUTER_BOUND('',#2172,.T.);
#1525=FACE_OUTER_BOUND('',#2174,.T.);
#1526=FACE_OUTER_BOUND('',#2175,.T.);
#1527=FACE_OUTER_BOUND('',#2176,.T.);
#1528=FACE_OUTER_BOUND('',#2178,.T.);
#1529=FACE_OUTER_BOUND('',#2180,.T.);
#1530=FACE_OUTER_BOUND('',#2181,.T.);
#1531=FACE_OUTER_BOUND('',#2182,.T.);
#1532=FACE_OUTER_BOUND('',#2184,.T.);
#1533=FACE_OUTER_BOUND('',#2185,.T.);
#1534=FACE_OUTER_BOUND('',#2186,.T.);
#1535=FACE_OUTER_BOUND('',#2187,.T.);
#1536=FACE_OUTER_BOUND('',#2188,.T.);
#1537=FACE_OUTER_BOUND('',#2189,.T.);
#1538=FACE_OUTER_BOUND('',#2190,.T.);
#1539=FACE_OUTER_BOUND('',#2191,.T.);
#1540=FACE_OUTER_BOUND('',#2192,.T.);
#1541=FACE_OUTER_BOUND('',#2193,.T.);
#1542=FACE_OUTER_BOUND('',#2194,.T.);
#1543=FACE_OUTER_BOUND('',#2195,.T.);
#1544=FACE_OUTER_BOUND('',#2196,.T.);
#1545=FACE_OUTER_BOUND('',#2197,.T.);
#1546=FACE_OUTER_BOUND('',#2198,.T.);
#1547=FACE_OUTER_BOUND('',#2200,.T.);
#1548=FACE_OUTER_BOUND('',#2202,.T.);
#1549=FACE_OUTER_BOUND('',#2203,.T.);
#1550=FACE_OUTER_BOUND('',#2204,.T.);
#1551=FACE_OUTER_BOUND('',#2205,.T.);
#1552=FACE_OUTER_BOUND('',#2207,.T.);
#1553=FACE_OUTER_BOUND('',#2209,.T.);
#1554=FACE_OUTER_BOUND('',#2211,.T.);
#1555=FACE_OUTER_BOUND('',#2212,.T.);
#1556=FACE_OUTER_BOUND('',#2213,.T.);
#1557=FACE_OUTER_BOUND('',#2214,.T.);
#1558=FACE_OUTER_BOUND('',#2215,.T.);
#1559=FACE_OUTER_BOUND('',#2216,.T.);
#1560=FACE_OUTER_BOUND('',#2217,.T.);
#1561=FACE_OUTER_BOUND('',#2218,.T.);
#1562=FACE_OUTER_BOUND('',#2219,.T.);
#1563=FACE_OUTER_BOUND('',#2220,.T.);
#1564=FACE_OUTER_BOUND('',#2221,.T.);
#1565=FACE_OUTER_BOUND('',#2222,.T.);
#1566=FACE_OUTER_BOUND('',#2223,.T.);
#1567=FACE_OUTER_BOUND('',#2224,.T.);
#1568=FACE_OUTER_BOUND('',#2225,.T.);
#1569=FACE_OUTER_BOUND('',#2227,.T.);
#1570=FACE_OUTER_BOUND('',#2228,.T.);
#1571=FACE_OUTER_BOUND('',#2229,.T.);
#1572=FACE_OUTER_BOUND('',#2230,.T.);
#1573=EDGE_LOOP('',(#5569,#5570,#5571,#5572));
#1574=EDGE_LOOP('',(#5573,#5574,#5575,#5576));
#1575=EDGE_LOOP('',(#5577,#5578,#5579,#5580));
#1576=EDGE_LOOP('',(#5581,#5582,#5583,#5584));
#1577=EDGE_LOOP('',(#5585,#5586,#5587,#5588));
#1578=EDGE_LOOP('',(#5589,#5590,#5591,#5592));
#1579=EDGE_LOOP('',(#5593,#5594,#5595,#5596));
#1580=EDGE_LOOP('',(#5597,#5598,#5599,#5600));
#1581=EDGE_LOOP('',(#5601,#5602,#5603,#5604));
#1582=EDGE_LOOP('',(#5605,#5606,#5607,#5608));
#1583=EDGE_LOOP('',(#5609,#5610,#5611,#5612));
#1584=EDGE_LOOP('',(#5613,#5614,#5615,#5616));
#1585=EDGE_LOOP('',(#5617,#5618,#5619,#5620));
#1586=EDGE_LOOP('',(#5621,#5622,#5623,#5624));
#1587=EDGE_LOOP('',(#5625,#5626,#5627,#5628));
#1588=EDGE_LOOP('',(#5629,#5630,#5631,#5632));
#1589=EDGE_LOOP('',(#5633,#5634,#5635,#5636));
#1590=EDGE_LOOP('',(#5637));
#1591=EDGE_LOOP('',(#5638));
#1592=EDGE_LOOP('',(#5639));
#1593=EDGE_LOOP('',(#5640));
#1594=EDGE_LOOP('',(#5641));
#1595=EDGE_LOOP('',(#5642));
#1596=EDGE_LOOP('',(#5643));
#1597=EDGE_LOOP('',(#5644));
#1598=EDGE_LOOP('',(#5645));
#1599=EDGE_LOOP('',(#5646));
#1600=EDGE_LOOP('',(#5647));
#1601=EDGE_LOOP('',(#5648));
#1602=EDGE_LOOP('',(#5649,#5650,#5651,#5652));
#1603=EDGE_LOOP('',(#5653));
#1604=EDGE_LOOP('',(#5654));
#1605=EDGE_LOOP('',(#5655));
#1606=EDGE_LOOP('',(#5656));
#1607=EDGE_LOOP('',(#5657));
#1608=EDGE_LOOP('',(#5658));
#1609=EDGE_LOOP('',(#5659));
#1610=EDGE_LOOP('',(#5660));
#1611=EDGE_LOOP('',(#5661));
#1612=EDGE_LOOP('',(#5662));
#1613=EDGE_LOOP('',(#5663));
#1614=EDGE_LOOP('',(#5664));
#1615=EDGE_LOOP('',(#5665,#5666,#5667,#5668));
#1616=EDGE_LOOP('',(#5669,#5670,#5671,#5672));
#1617=EDGE_LOOP('',(#5673,#5674,#5675,#5676));
#1618=EDGE_LOOP('',(#5677,#5678,#5679,#5680));
#1619=EDGE_LOOP('',(#5681,#5682,#5683,#5684));
#1620=EDGE_LOOP('',(#5685,#5686,#5687,#5688));
#1621=EDGE_LOOP('',(#5689,#5690,#5691,#5692));
#1622=EDGE_LOOP('',(#5693,#5694,#5695,#5696));
#1623=EDGE_LOOP('',(#5697,#5698,#5699,#5700));
#1624=EDGE_LOOP('',(#5701));
#1625=EDGE_LOOP('',(#5702));
#1626=EDGE_LOOP('',(#5703));
#1627=EDGE_LOOP('',(#5704));
#1628=EDGE_LOOP('',(#5705,#5706,#5707,#5708));
#1629=EDGE_LOOP('',(#5709));
#1630=EDGE_LOOP('',(#5710));
#1631=EDGE_LOOP('',(#5711));
#1632=EDGE_LOOP('',(#5712));
#1633=EDGE_LOOP('',(#5713,#5714,#5715,#5716));
#1634=EDGE_LOOP('',(#5717,#5718,#5719,#5720));
#1635=EDGE_LOOP('',(#5721,#5722,#5723,#5724));
#1636=EDGE_LOOP('',(#5725,#5726,#5727,#5728));
#1637=EDGE_LOOP('',(#5729,#5730,#5731,#5732));
#1638=EDGE_LOOP('',(#5733,#5734,#5735,#5736));
#1639=EDGE_LOOP('',(#5737,#5738,#5739,#5740));
#1640=EDGE_LOOP('',(#5741,#5742,#5743,#5744));
#1641=EDGE_LOOP('',(#5745,#5746,#5747,#5748));
#1642=EDGE_LOOP('',(#5749,#5750,#5751,#5752));
#1643=EDGE_LOOP('',(#5753,#5754,#5755,#5756));
#1644=EDGE_LOOP('',(#5757,#5758,#5759,#5760));
#1645=EDGE_LOOP('',(#5761,#5762,#5763,#5764));
#1646=EDGE_LOOP('',(#5765,#5766,#5767,#5768));
#1647=EDGE_LOOP('',(#5769));
#1648=EDGE_LOOP('',(#5770,#5771,#5772,#5773));
#1649=EDGE_LOOP('',(#5774));
#1650=EDGE_LOOP('',(#5775,#5776,#5777,#5778));
#1651=EDGE_LOOP('',(#5779));
#1652=EDGE_LOOP('',(#5780,#5781,#5782,#5783));
#1653=EDGE_LOOP('',(#5784));
#1654=EDGE_LOOP('',(#5785,#5786,#5787,#5788));
#1655=EDGE_LOOP('',(#5789,#5790,#5791,#5792));
#1656=EDGE_LOOP('',(#5793,#5794,#5795,#5796));
#1657=EDGE_LOOP('',(#5797,#5798,#5799,#5800));
#1658=EDGE_LOOP('',(#5801,#5802,#5803,#5804));
#1659=EDGE_LOOP('',(#5805,#5806,#5807,#5808));
#1660=EDGE_LOOP('',(#5809,#5810,#5811,#5812));
#1661=EDGE_LOOP('',(#5813,#5814,#5815,#5816));
#1662=EDGE_LOOP('',(#5817,#5818,#5819,#5820));
#1663=EDGE_LOOP('',(#5821));
#1664=EDGE_LOOP('',(#5822));
#1665=EDGE_LOOP('',(#5823,#5824,#5825,#5826));
#1666=EDGE_LOOP('',(#5827,#5828,#5829,#5830));
#1667=EDGE_LOOP('',(#5831,#5832,#5833,#5834));
#1668=EDGE_LOOP('',(#5835,#5836,#5837,#5838,#5839,#5840,#5841,#5842,#5843,
#5844));
#1669=EDGE_LOOP('',(#5845));
#1670=EDGE_LOOP('',(#5846));
#1671=EDGE_LOOP('',(#5847));
#1672=EDGE_LOOP('',(#5848));
#1673=EDGE_LOOP('',(#5849));
#1674=EDGE_LOOP('',(#5850));
#1675=EDGE_LOOP('',(#5851,#5852,#5853,#5854));
#1676=EDGE_LOOP('',(#5855));
#1677=EDGE_LOOP('',(#5856));
#1678=EDGE_LOOP('',(#5857));
#1679=EDGE_LOOP('',(#5858));
#1680=EDGE_LOOP('',(#5859));
#1681=EDGE_LOOP('',(#5860,#5861,#5862,#5863));
#1682=EDGE_LOOP('',(#5864,#5865,#5866,#5867));
#1683=EDGE_LOOP('',(#5868));
#1684=EDGE_LOOP('',(#5869));
#1685=EDGE_LOOP('',(#5870));
#1686=EDGE_LOOP('',(#5871));
#1687=EDGE_LOOP('',(#5872,#5873,#5874,#5875));
#1688=EDGE_LOOP('',(#5876,#5877,#5878,#5879));
#1689=EDGE_LOOP('',(#5880,#5881,#5882,#5883));
#1690=EDGE_LOOP('',(#5884,#5885,#5886,#5887));
#1691=EDGE_LOOP('',(#5888,#5889,#5890,#5891));
#1692=EDGE_LOOP('',(#5892,#5893,#5894,#5895));
#1693=EDGE_LOOP('',(#5896,#5897,#5898,#5899,#5900,#5901,#5902,#5903,#5904,
#5905));
#1694=EDGE_LOOP('',(#5906));
#1695=EDGE_LOOP('',(#5907));
#1696=EDGE_LOOP('',(#5908));
#1697=EDGE_LOOP('',(#5909));
#1698=EDGE_LOOP('',(#5910));
#1699=EDGE_LOOP('',(#5911));
#1700=EDGE_LOOP('',(#5912,#5913,#5914,#5915));
#1701=EDGE_LOOP('',(#5916,#5917,#5918,#5919));
#1702=EDGE_LOOP('',(#5920));
#1703=EDGE_LOOP('',(#5921,#5922,#5923,#5924));
#1704=EDGE_LOOP('',(#5925,#5926,#5927,#5928));
#1705=EDGE_LOOP('',(#5929,#5930,#5931,#5932));
#1706=EDGE_LOOP('',(#5933,#5934,#5935,#5936));
#1707=EDGE_LOOP('',(#5937));
#1708=EDGE_LOOP('',(#5938));
#1709=EDGE_LOOP('',(#5939));
#1710=EDGE_LOOP('',(#5940));
#1711=EDGE_LOOP('',(#5941,#5942,#5943,#5944));
#1712=EDGE_LOOP('',(#5945,#5946,#5947,#5948));
#1713=EDGE_LOOP('',(#5949,#5950,#5951,#5952));
#1714=EDGE_LOOP('',(#5953,#5954,#5955,#5956));
#1715=EDGE_LOOP('',(#5957,#5958,#5959,#5960));
#1716=EDGE_LOOP('',(#5961));
#1717=EDGE_LOOP('',(#5962));
#1718=EDGE_LOOP('',(#5963,#5964,#5965,#5966));
#1719=EDGE_LOOP('',(#5967,#5968,#5969,#5970));
#1720=EDGE_LOOP('',(#5971));
#1721=EDGE_LOOP('',(#5972));
#1722=EDGE_LOOP('',(#5973));
#1723=EDGE_LOOP('',(#5974));
#1724=EDGE_LOOP('',(#5975));
#1725=EDGE_LOOP('',(#5976));
#1726=EDGE_LOOP('',(#5977));
#1727=EDGE_LOOP('',(#5978));
#1728=EDGE_LOOP('',(#5979));
#1729=EDGE_LOOP('',(#5980));
#1730=EDGE_LOOP('',(#5981));
#1731=EDGE_LOOP('',(#5982));
#1732=EDGE_LOOP('',(#5983,#5984,#5985,#5986));
#1733=EDGE_LOOP('',(#5987,#5988,#5989,#5990));
#1734=EDGE_LOOP('',(#5991,#5992,#5993,#5994));
#1735=EDGE_LOOP('',(#5995,#5996,#5997,#5998));
#1736=EDGE_LOOP('',(#5999,#6000,#6001,#6002));
#1737=EDGE_LOOP('',(#6003));
#1738=EDGE_LOOP('',(#6004));
#1739=EDGE_LOOP('',(#6005,#6006,#6007,#6008));
#1740=EDGE_LOOP('',(#6009,#6010,#6011,#6012));
#1741=EDGE_LOOP('',(#6013));
#1742=EDGE_LOOP('',(#6014));
#1743=EDGE_LOOP('',(#6015));
#1744=EDGE_LOOP('',(#6016));
#1745=EDGE_LOOP('',(#6017));
#1746=EDGE_LOOP('',(#6018));
#1747=EDGE_LOOP('',(#6019));
#1748=EDGE_LOOP('',(#6020));
#1749=EDGE_LOOP('',(#6021));
#1750=EDGE_LOOP('',(#6022));
#1751=EDGE_LOOP('',(#6023));
#1752=EDGE_LOOP('',(#6024));
#1753=EDGE_LOOP('',(#6025,#6026,#6027,#6028));
#1754=EDGE_LOOP('',(#6029));
#1755=EDGE_LOOP('',(#6030));
#1756=EDGE_LOOP('',(#6031,#6032,#6033,#6034));
#1757=EDGE_LOOP('',(#6035));
#1758=EDGE_LOOP('',(#6036));
#1759=EDGE_LOOP('',(#6037,#6038,#6039,#6040));
#1760=EDGE_LOOP('',(#6041));
#1761=EDGE_LOOP('',(#6042));
#1762=EDGE_LOOP('',(#6043,#6044,#6045,#6046));
#1763=EDGE_LOOP('',(#6047));
#1764=EDGE_LOOP('',(#6048));
#1765=EDGE_LOOP('',(#6049,#6050,#6051,#6052));
#1766=EDGE_LOOP('',(#6053,#6054,#6055,#6056));
#1767=EDGE_LOOP('',(#6057,#6058,#6059,#6060));
#1768=EDGE_LOOP('',(#6061,#6062,#6063,#6064));
#1769=EDGE_LOOP('',(#6065,#6066,#6067,#6068));
#1770=EDGE_LOOP('',(#6069));
#1771=EDGE_LOOP('',(#6070));
#1772=EDGE_LOOP('',(#6071,#6072,#6073,#6074));
#1773=EDGE_LOOP('',(#6075,#6076,#6077,#6078));
#1774=EDGE_LOOP('',(#6079));
#1775=EDGE_LOOP('',(#6080));
#1776=EDGE_LOOP('',(#6081));
#1777=EDGE_LOOP('',(#6082));
#1778=EDGE_LOOP('',(#6083));
#1779=EDGE_LOOP('',(#6084));
#1780=EDGE_LOOP('',(#6085));
#1781=EDGE_LOOP('',(#6086));
#1782=EDGE_LOOP('',(#6087));
#1783=EDGE_LOOP('',(#6088));
#1784=EDGE_LOOP('',(#6089));
#1785=EDGE_LOOP('',(#6090));
#1786=EDGE_LOOP('',(#6091,#6092,#6093,#6094));
#1787=EDGE_LOOP('',(#6095,#6096,#6097,#6098));
#1788=EDGE_LOOP('',(#6099,#6100,#6101,#6102));
#1789=EDGE_LOOP('',(#6103,#6104,#6105,#6106));
#1790=EDGE_LOOP('',(#6107,#6108,#6109,#6110));
#1791=EDGE_LOOP('',(#6111,#6112,#6113,#6114));
#1792=EDGE_LOOP('',(#6115,#6116,#6117,#6118));
#1793=EDGE_LOOP('',(#6119));
#1794=EDGE_LOOP('',(#6120,#6121,#6122,#6123));
#1795=EDGE_LOOP('',(#6124));
#1796=EDGE_LOOP('',(#6125,#6126,#6127,#6128));
#1797=EDGE_LOOP('',(#6129,#6130,#6131,#6132));
#1798=EDGE_LOOP('',(#6133,#6134,#6135,#6136));
#1799=EDGE_LOOP('',(#6137,#6138,#6139,#6140));
#1800=EDGE_LOOP('',(#6141,#6142,#6143,#6144));
#1801=EDGE_LOOP('',(#6145,#6146,#6147,#6148));
#1802=EDGE_LOOP('',(#6149));
#1803=EDGE_LOOP('',(#6150));
#1804=EDGE_LOOP('',(#6151,#6152,#6153,#6154));
#1805=EDGE_LOOP('',(#6155));
#1806=EDGE_LOOP('',(#6156,#6157,#6158,#6159));
#1807=EDGE_LOOP('',(#6160));
#1808=EDGE_LOOP('',(#6161,#6162,#6163,#6164));
#1809=EDGE_LOOP('',(#6165,#6166,#6167,#6168));
#1810=EDGE_LOOP('',(#6169,#6170,#6171,#6172));
#1811=EDGE_LOOP('',(#6173,#6174,#6175,#6176));
#1812=EDGE_LOOP('',(#6177,#6178,#6179,#6180));
#1813=EDGE_LOOP('',(#6181,#6182,#6183,#6184));
#1814=EDGE_LOOP('',(#6185));
#1815=EDGE_LOOP('',(#6186));
#1816=EDGE_LOOP('',(#6187,#6188,#6189,#6190));
#1817=EDGE_LOOP('',(#6191));
#1818=EDGE_LOOP('',(#6192));
#1819=EDGE_LOOP('',(#6193));
#1820=EDGE_LOOP('',(#6194,#6195,#6196,#6197));
#1821=EDGE_LOOP('',(#6198));
#1822=EDGE_LOOP('',(#6199));
#1823=EDGE_LOOP('',(#6200,#6201,#6202,#6203));
#1824=EDGE_LOOP('',(#6204));
#1825=EDGE_LOOP('',(#6205,#6206,#6207,#6208));
#1826=EDGE_LOOP('',(#6209,#6210,#6211,#6212));
#1827=EDGE_LOOP('',(#6213,#6214,#6215,#6216));
#1828=EDGE_LOOP('',(#6217,#6218,#6219,#6220));
#1829=EDGE_LOOP('',(#6221,#6222,#6223,#6224));
#1830=EDGE_LOOP('',(#6225,#6226,#6227,#6228));
#1831=EDGE_LOOP('',(#6229,#6230,#6231,#6232));
#1832=EDGE_LOOP('',(#6233,#6234,#6235,#6236));
#1833=EDGE_LOOP('',(#6237,#6238,#6239,#6240));
#1834=EDGE_LOOP('',(#6241,#6242,#6243,#6244));
#1835=EDGE_LOOP('',(#6245,#6246,#6247,#6248));
#1836=EDGE_LOOP('',(#6249,#6250,#6251,#6252));
#1837=EDGE_LOOP('',(#6253,#6254,#6255,#6256));
#1838=EDGE_LOOP('',(#6257,#6258,#6259,#6260));
#1839=EDGE_LOOP('',(#6261,#6262,#6263,#6264));
#1840=EDGE_LOOP('',(#6265,#6266,#6267,#6268));
#1841=EDGE_LOOP('',(#6269,#6270,#6271,#6272));
#1842=EDGE_LOOP('',(#6273,#6274,#6275,#6276));
#1843=EDGE_LOOP('',(#6277,#6278,#6279,#6280));
#1844=EDGE_LOOP('',(#6281,#6282,#6283,#6284));
#1845=EDGE_LOOP('',(#6285,#6286,#6287,#6288));
#1846=EDGE_LOOP('',(#6289,#6290,#6291,#6292));
#1847=EDGE_LOOP('',(#6293,#6294,#6295,#6296));
#1848=EDGE_LOOP('',(#6297,#6298,#6299,#6300));
#1849=EDGE_LOOP('',(#6301,#6302,#6303,#6304));
#1850=EDGE_LOOP('',(#6305,#6306,#6307,#6308));
#1851=EDGE_LOOP('',(#6309,#6310,#6311,#6312));
#1852=EDGE_LOOP('',(#6313,#6314,#6315,#6316));
#1853=EDGE_LOOP('',(#6317,#6318,#6319,#6320));
#1854=EDGE_LOOP('',(#6321,#6322,#6323,#6324));
#1855=EDGE_LOOP('',(#6325,#6326,#6327,#6328));
#1856=EDGE_LOOP('',(#6329,#6330,#6331,#6332));
#1857=EDGE_LOOP('',(#6333,#6334,#6335,#6336));
#1858=EDGE_LOOP('',(#6337,#6338,#6339,#6340));
#1859=EDGE_LOOP('',(#6341,#6342,#6343,#6344));
#1860=EDGE_LOOP('',(#6345,#6346,#6347,#6348));
#1861=EDGE_LOOP('',(#6349,#6350,#6351,#6352));
#1862=EDGE_LOOP('',(#6353,#6354,#6355,#6356));
#1863=EDGE_LOOP('',(#6357,#6358,#6359,#6360));
#1864=EDGE_LOOP('',(#6361,#6362,#6363,#6364));
#1865=EDGE_LOOP('',(#6365,#6366,#6367,#6368));
#1866=EDGE_LOOP('',(#6369,#6370,#6371,#6372));
#1867=EDGE_LOOP('',(#6373,#6374,#6375,#6376));
#1868=EDGE_LOOP('',(#6377,#6378,#6379,#6380));
#1869=EDGE_LOOP('',(#6381,#6382,#6383,#6384));
#1870=EDGE_LOOP('',(#6385,#6386,#6387,#6388,#6389,#6390,#6391,#6392,#6393,
#6394,#6395,#6396,#6397,#6398,#6399,#6400,#6401,#6402,#6403,#6404,#6405,
#6406,#6407,#6408,#6409,#6410,#6411,#6412,#6413,#6414,#6415,#6416,#6417,
#6418,#6419,#6420,#6421,#6422,#6423,#6424,#6425,#6426,#6427,#6428));
#1871=EDGE_LOOP('',(#6429));
#1872=EDGE_LOOP('',(#6430,#6431,#6432,#6433,#6434,#6435,#6436,#6437,#6438,
#6439,#6440,#6441,#6442,#6443,#6444,#6445,#6446,#6447,#6448,#6449,#6450,
#6451,#6452,#6453,#6454,#6455,#6456,#6457,#6458,#6459,#6460,#6461,#6462,
#6463,#6464,#6465,#6466,#6467,#6468,#6469,#6470,#6471,#6472,#6473));
#1873=EDGE_LOOP('',(#6474));
#1874=EDGE_LOOP('',(#6475,#6476,#6477,#6478));
#1875=EDGE_LOOP('',(#6479,#6480,#6481,#6482));
#1876=EDGE_LOOP('',(#6483,#6484,#6485,#6486));
#1877=EDGE_LOOP('',(#6487));
#1878=EDGE_LOOP('',(#6488,#6489,#6490,#6491,#6492,#6493,#6494,#6495,#6496,
#6497));
#1879=EDGE_LOOP('',(#6498,#6499,#6500,#6501));
#1880=EDGE_LOOP('',(#6502,#6503,#6504,#6505));
#1881=EDGE_LOOP('',(#6506,#6507,#6508,#6509,#6510,#6511,#6512,#6513,#6514,
#6515));
#1882=EDGE_LOOP('',(#6516,#6517,#6518,#6519));
#1883=EDGE_LOOP('',(#6520,#6521,#6522,#6523,#6524,#6525));
#1884=EDGE_LOOP('',(#6526,#6527,#6528,#6529,#6530,#6531,#6532,#6533));
#1885=EDGE_LOOP('',(#6534,#6535,#6536,#6537,#6538));
#1886=EDGE_LOOP('',(#6539,#6540,#6541,#6542));
#1887=EDGE_LOOP('',(#6543,#6544,#6545,#6546,#6547,#6548));
#1888=EDGE_LOOP('',(#6549,#6550,#6551,#6552));
#1889=EDGE_LOOP('',(#6553,#6554,#6555,#6556));
#1890=EDGE_LOOP('',(#6557,#6558,#6559,#6560));
#1891=EDGE_LOOP('',(#6561));
#1892=EDGE_LOOP('',(#6562));
#1893=EDGE_LOOP('',(#6563,#6564,#6565,#6566));
#1894=EDGE_LOOP('',(#6567));
#1895=EDGE_LOOP('',(#6568));
#1896=EDGE_LOOP('',(#6569,#6570,#6571,#6572));
#1897=EDGE_LOOP('',(#6573,#6574,#6575,#6576));
#1898=EDGE_LOOP('',(#6577,#6578,#6579,#6580));
#1899=EDGE_LOOP('',(#6581,#6582,#6583,#6584));
#1900=EDGE_LOOP('',(#6585,#6586,#6587,#6588));
#1901=EDGE_LOOP('',(#6589,#6590,#6591,#6592));
#1902=EDGE_LOOP('',(#6593,#6594,#6595,#6596,#6597,#6598));
#1903=EDGE_LOOP('',(#6599,#6600,#6601,#6602,#6603,#6604));
#1904=EDGE_LOOP('',(#6605));
#1905=EDGE_LOOP('',(#6606));
#1906=EDGE_LOOP('',(#6607,#6608,#6609,#6610));
#1907=EDGE_LOOP('',(#6611,#6612,#6613,#6614));
#1908=EDGE_LOOP('',(#6615,#6616,#6617,#6618));
#1909=EDGE_LOOP('',(#6619));
#1910=EDGE_LOOP('',(#6620));
#1911=EDGE_LOOP('',(#6621,#6622,#6623,#6624));
#1912=EDGE_LOOP('',(#6625,#6626,#6627,#6628));
#1913=EDGE_LOOP('',(#6629,#6630,#6631,#6632,#6633,#6634));
#1914=EDGE_LOOP('',(#6635,#6636,#6637,#6638,#6639));
#1915=EDGE_LOOP('',(#6640,#6641,#6642,#6643));
#1916=EDGE_LOOP('',(#6644,#6645,#6646,#6647));
#1917=EDGE_LOOP('',(#6648));
#1918=EDGE_LOOP('',(#6649));
#1919=EDGE_LOOP('',(#6650,#6651,#6652,#6653,#6654));
#1920=EDGE_LOOP('',(#6655));
#1921=EDGE_LOOP('',(#6656));
#1922=EDGE_LOOP('',(#6657,#6658,#6659,#6660));
#1923=EDGE_LOOP('',(#6661,#6662,#6663,#6664,#6665,#6666));
#1924=EDGE_LOOP('',(#6667,#6668,#6669,#6670,#6671));
#1925=EDGE_LOOP('',(#6672));
#1926=EDGE_LOOP('',(#6673));
#1927=EDGE_LOOP('',(#6674,#6675,#6676,#6677));
#1928=EDGE_LOOP('',(#6678,#6679,#6680,#6681));
#1929=EDGE_LOOP('',(#6682,#6683,#6684,#6685));
#1930=EDGE_LOOP('',(#6686));
#1931=EDGE_LOOP('',(#6687));
#1932=EDGE_LOOP('',(#6688,#6689,#6690,#6691,#6692));
#1933=EDGE_LOOP('',(#6693,#6694));
#1934=EDGE_LOOP('',(#6695,#6696));
#1935=EDGE_LOOP('',(#6697,#6698));
#1936=EDGE_LOOP('',(#6699,#6700));
#1937=EDGE_LOOP('',(#6701,#6702));
#1938=EDGE_LOOP('',(#6703,#6704));
#1939=EDGE_LOOP('',(#6705,#6706));
#1940=EDGE_LOOP('',(#6707,#6708));
#1941=EDGE_LOOP('',(#6709,#6710,#6711,#6712));
#1942=EDGE_LOOP('',(#6713,#6714,#6715,#6716,#6717,#6718,#6719,#6720,#6721,
#6722,#6723,#6724,#6725,#6726,#6727,#6728,#6729,#6730,#6731,#6732));
#1943=EDGE_LOOP('',(#6733,#6734,#6735,#6736));
#1944=EDGE_LOOP('',(#6737,#6738,#6739,#6740));
#1945=EDGE_LOOP('',(#6741,#6742,#6743,#6744));
#1946=EDGE_LOOP('',(#6745,#6746,#6747,#6748));
#1947=EDGE_LOOP('',(#6749,#6750,#6751,#6752));
#1948=EDGE_LOOP('',(#6753,#6754,#6755,#6756,#6757,#6758));
#1949=EDGE_LOOP('',(#6759,#6760,#6761,#6762));
#1950=EDGE_LOOP('',(#6763,#6764,#6765,#6766));
#1951=EDGE_LOOP('',(#6767,#6768,#6769,#6770));
#1952=EDGE_LOOP('',(#6771,#6772,#6773,#6774));
#1953=EDGE_LOOP('',(#6775,#6776,#6777,#6778));
#1954=EDGE_LOOP('',(#6779,#6780,#6781,#6782));
#1955=EDGE_LOOP('',(#6783,#6784,#6785,#6786,#6787,#6788,#6789,#6790,#6791,
#6792,#6793,#6794,#6795,#6796,#6797,#6798,#6799,#6800,#6801,#6802));
#1956=EDGE_LOOP('',(#6803,#6804,#6805,#6806));
#1957=EDGE_LOOP('',(#6807,#6808,#6809,#6810));
#1958=EDGE_LOOP('',(#6811));
#1959=EDGE_LOOP('',(#6812));
#1960=EDGE_LOOP('',(#6813,#6814,#6815,#6816));
#1961=EDGE_LOOP('',(#6817));
#1962=EDGE_LOOP('',(#6818));
#1963=EDGE_LOOP('',(#6819,#6820,#6821,#6822));
#1964=EDGE_LOOP('',(#6823));
#1965=EDGE_LOOP('',(#6824));
#1966=EDGE_LOOP('',(#6825,#6826,#6827,#6828));
#1967=EDGE_LOOP('',(#6829));
#1968=EDGE_LOOP('',(#6830));
#1969=EDGE_LOOP('',(#6831,#6832,#6833,#6834));
#1970=EDGE_LOOP('',(#6835));
#1971=EDGE_LOOP('',(#6836));
#1972=EDGE_LOOP('',(#6837,#6838,#6839,#6840));
#1973=EDGE_LOOP('',(#6841,#6842,#6843,#6844));
#1974=EDGE_LOOP('',(#6845,#6846,#6847,#6848));
#1975=EDGE_LOOP('',(#6849,#6850,#6851,#6852));
#1976=EDGE_LOOP('',(#6853,#6854,#6855,#6856));
#1977=EDGE_LOOP('',(#6857,#6858,#6859,#6860));
#1978=EDGE_LOOP('',(#6861));
#1979=EDGE_LOOP('',(#6862));
#1980=EDGE_LOOP('',(#6863,#6864,#6865,#6866));
#1981=EDGE_LOOP('',(#6867));
#1982=EDGE_LOOP('',(#6868));
#1983=EDGE_LOOP('',(#6869,#6870,#6871,#6872));
#1984=EDGE_LOOP('',(#6873));
#1985=EDGE_LOOP('',(#6874));
#1986=EDGE_LOOP('',(#6875,#6876,#6877,#6878));
#1987=EDGE_LOOP('',(#6879));
#1988=EDGE_LOOP('',(#6880));
#1989=EDGE_LOOP('',(#6881,#6882,#6883,#6884));
#1990=EDGE_LOOP('',(#6885));
#1991=EDGE_LOOP('',(#6886));
#1992=EDGE_LOOP('',(#6887,#6888,#6889,#6890));
#1993=EDGE_LOOP('',(#6891));
#1994=EDGE_LOOP('',(#6892));
#1995=EDGE_LOOP('',(#6893,#6894,#6895,#6896));
#1996=EDGE_LOOP('',(#6897,#6898,#6899,#6900));
#1997=EDGE_LOOP('',(#6901,#6902,#6903,#6904));
#1998=EDGE_LOOP('',(#6905,#6906,#6907,#6908));
#1999=EDGE_LOOP('',(#6909,#6910,#6911,#6912));
#2000=EDGE_LOOP('',(#6913,#6914,#6915,#6916));
#2001=EDGE_LOOP('',(#6917));
#2002=EDGE_LOOP('',(#6918));
#2003=EDGE_LOOP('',(#6919,#6920,#6921,#6922));
#2004=EDGE_LOOP('',(#6923,#6924,#6925,#6926));
#2005=EDGE_LOOP('',(#6927));
#2006=EDGE_LOOP('',(#6928));
#2007=EDGE_LOOP('',(#6929,#6930,#6931,#6932));
#2008=EDGE_LOOP('',(#6933,#6934,#6935,#6936));
#2009=EDGE_LOOP('',(#6937,#6938,#6939,#6940));
#2010=EDGE_LOOP('',(#6941,#6942,#6943,#6944));
#2011=EDGE_LOOP('',(#6945,#6946,#6947,#6948));
#2012=EDGE_LOOP('',(#6949,#6950,#6951,#6952));
#2013=EDGE_LOOP('',(#6953,#6954,#6955,#6956));
#2014=EDGE_LOOP('',(#6957,#6958,#6959,#6960));
#2015=EDGE_LOOP('',(#6961,#6962,#6963,#6964,#6965,#6966));
#2016=EDGE_LOOP('',(#6967,#6968,#6969,#6970,#6971,#6972));
#2017=EDGE_LOOP('',(#6973));
#2018=EDGE_LOOP('',(#6974));
#2019=EDGE_LOOP('',(#6975,#6976,#6977,#6978));
#2020=EDGE_LOOP('',(#6979));
#2021=EDGE_LOOP('',(#6980));
#2022=EDGE_LOOP('',(#6981,#6982,#6983,#6984));
#2023=EDGE_LOOP('',(#6985,#6986,#6987,#6988));
#2024=EDGE_LOOP('',(#6989,#6990,#6991,#6992));
#2025=EDGE_LOOP('',(#6993));
#2026=EDGE_LOOP('',(#6994));
#2027=EDGE_LOOP('',(#6995,#6996,#6997,#6998));
#2028=EDGE_LOOP('',(#6999,#7000,#7001,#7002));
#2029=EDGE_LOOP('',(#7003,#7004,#7005,#7006));
#2030=EDGE_LOOP('',(#7007,#7008,#7009,#7010));
#2031=EDGE_LOOP('',(#7011,#7012,#7013,#7014));
#2032=EDGE_LOOP('',(#7015,#7016,#7017,#7018,#7019,#7020,#7021,#7022,#7023));
#2033=EDGE_LOOP('',(#7024));
#2034=EDGE_LOOP('',(#7025));
#2035=EDGE_LOOP('',(#7026,#7027,#7028,#7029));
#2036=EDGE_LOOP('',(#7030,#7031,#7032,#7033));
#2037=EDGE_LOOP('',(#7034,#7035,#7036,#7037));
#2038=EDGE_LOOP('',(#7038,#7039,#7040,#7041));
#2039=EDGE_LOOP('',(#7042,#7043,#7044,#7045));
#2040=EDGE_LOOP('',(#7046,#7047,#7048,#7049));
#2041=EDGE_LOOP('',(#7050));
#2042=EDGE_LOOP('',(#7051,#7052,#7053,#7054));
#2043=EDGE_LOOP('',(#7055));
#2044=EDGE_LOOP('',(#7056));
#2045=EDGE_LOOP('',(#7057,#7058,#7059,#7060,#7061,#7062,#7063,#7064,#7065,
#7066,#7067,#7068));
#2046=EDGE_LOOP('',(#7069));
#2047=EDGE_LOOP('',(#7070));
#2048=EDGE_LOOP('',(#7071,#7072,#7073,#7074));
#2049=EDGE_LOOP('',(#7075,#7076,#7077,#7078));
#2050=EDGE_LOOP('',(#7079,#7080,#7081,#7082));
#2051=EDGE_LOOP('',(#7083));
#2052=EDGE_LOOP('',(#7084));
#2053=EDGE_LOOP('',(#7085,#7086,#7087,#7088));
#2054=EDGE_LOOP('',(#7089,#7090,#7091,#7092));
#2055=EDGE_LOOP('',(#7093));
#2056=EDGE_LOOP('',(#7094));
#2057=EDGE_LOOP('',(#7095));
#2058=EDGE_LOOP('',(#7096));
#2059=EDGE_LOOP('',(#7097,#7098));
#2060=EDGE_LOOP('',(#7099,#7100,#7101,#7102,#7103,#7104,#7105,#7106,#7107));
#2061=EDGE_LOOP('',(#7108,#7109,#7110));
#2062=EDGE_LOOP('',(#7111,#7112,#7113,#7114));
#2063=EDGE_LOOP('',(#7115,#7116,#7117,#7118));
#2064=EDGE_LOOP('',(#7119,#7120,#7121,#7122));
#2065=EDGE_LOOP('',(#7123,#7124));
#2066=EDGE_LOOP('',(#7125));
#2067=EDGE_LOOP('',(#7126));
#2068=EDGE_LOOP('',(#7127));
#2069=EDGE_LOOP('',(#7128));
#2070=EDGE_LOOP('',(#7129,#7130,#7131,#7132));
#2071=EDGE_LOOP('',(#7133));
#2072=EDGE_LOOP('',(#7134,#7135,#7136,#7137));
#2073=EDGE_LOOP('',(#7138));
#2074=EDGE_LOOP('',(#7139));
#2075=EDGE_LOOP('',(#7140));
#2076=EDGE_LOOP('',(#7141));
#2077=EDGE_LOOP('',(#7142));
#2078=EDGE_LOOP('',(#7143,#7144,#7145,#7146));
#2079=EDGE_LOOP('',(#7147,#7148,#7149,#7150));
#2080=EDGE_LOOP('',(#7151,#7152,#7153,#7154));
#2081=EDGE_LOOP('',(#7155));
#2082=EDGE_LOOP('',(#7156));
#2083=EDGE_LOOP('',(#7157));
#2084=EDGE_LOOP('',(#7158));
#2085=EDGE_LOOP('',(#7159,#7160,#7161,#7162));
#2086=EDGE_LOOP('',(#7163,#7164,#7165,#7166));
#2087=EDGE_LOOP('',(#7167));
#2088=EDGE_LOOP('',(#7168));
#2089=EDGE_LOOP('',(#7169));
#2090=EDGE_LOOP('',(#7170));
#2091=EDGE_LOOP('',(#7171,#7172,#7173,#7174));
#2092=EDGE_LOOP('',(#7175,#7176,#7177,#7178));
#2093=EDGE_LOOP('',(#7179));
#2094=EDGE_LOOP('',(#7180));
#2095=EDGE_LOOP('',(#7181));
#2096=EDGE_LOOP('',(#7182));
#2097=EDGE_LOOP('',(#7183,#7184,#7185,#7186));
#2098=EDGE_LOOP('',(#7187,#7188,#7189,#7190));
#2099=EDGE_LOOP('',(#7191));
#2100=EDGE_LOOP('',(#7192));
#2101=EDGE_LOOP('',(#7193));
#2102=EDGE_LOOP('',(#7194));
#2103=EDGE_LOOP('',(#7195,#7196,#7197,#7198));
#2104=EDGE_LOOP('',(#7199,#7200,#7201,#7202));
#2105=EDGE_LOOP('',(#7203));
#2106=EDGE_LOOP('',(#7204));
#2107=EDGE_LOOP('',(#7205));
#2108=EDGE_LOOP('',(#7206));
#2109=EDGE_LOOP('',(#7207));
#2110=EDGE_LOOP('',(#7208,#7209,#7210,#7211));
#2111=EDGE_LOOP('',(#7212,#7213,#7214,#7215));
#2112=EDGE_LOOP('',(#7216,#7217,#7218,#7219));
#2113=EDGE_LOOP('',(#7220,#7221,#7222,#7223));
#2114=EDGE_LOOP('',(#7224,#7225,#7226,#7227));
#2115=EDGE_LOOP('',(#7228,#7229,#7230,#7231));
#2116=EDGE_LOOP('',(#7232,#7233,#7234,#7235,#7236,#7237));
#2117=EDGE_LOOP('',(#7238));
#2118=EDGE_LOOP('',(#7239,#7240,#7241,#7242,#7243,#7244));
#2119=EDGE_LOOP('',(#7245,#7246,#7247,#7248));
#2120=EDGE_LOOP('',(#7249,#7250,#7251,#7252));
#2121=EDGE_LOOP('',(#7253,#7254,#7255,#7256));
#2122=EDGE_LOOP('',(#7257,#7258,#7259,#7260));
#2123=EDGE_LOOP('',(#7261,#7262,#7263,#7264));
#2124=EDGE_LOOP('',(#7265,#7266,#7267,#7268));
#2125=EDGE_LOOP('',(#7269,#7270,#7271,#7272));
#2126=EDGE_LOOP('',(#7273,#7274,#7275,#7276));
#2127=EDGE_LOOP('',(#7277,#7278,#7279,#7280,#7281,#7282));
#2128=EDGE_LOOP('',(#7283,#7284,#7285,#7286,#7287,#7288));
#2129=EDGE_LOOP('',(#7289));
#2130=EDGE_LOOP('',(#7290));
#2131=EDGE_LOOP('',(#7291,#7292,#7293,#7294));
#2132=EDGE_LOOP('',(#7295,#7296,#7297,#7298));
#2133=EDGE_LOOP('',(#7299,#7300,#7301,#7302));
#2134=EDGE_LOOP('',(#7303));
#2135=EDGE_LOOP('',(#7304));
#2136=EDGE_LOOP('',(#7305,#7306,#7307,#7308));
#2137=EDGE_LOOP('',(#7309,#7310,#7311,#7312));
#2138=EDGE_LOOP('',(#7313));
#2139=EDGE_LOOP('',(#7314,#7315,#7316,#7317));
#2140=EDGE_LOOP('',(#7318,#7319,#7320,#7321));
#2141=EDGE_LOOP('',(#7322,#7323,#7324,#7325));
#2142=EDGE_LOOP('',(#7326));
#2143=EDGE_LOOP('',(#7327));
#2144=EDGE_LOOP('',(#7328,#7329,#7330,#7331));
#2145=EDGE_LOOP('',(#7332,#7333,#7334,#7335));
#2146=EDGE_LOOP('',(#7336,#7337,#7338,#7339));
#2147=EDGE_LOOP('',(#7340));
#2148=EDGE_LOOP('',(#7341,#7342,#7343,#7344));
#2149=EDGE_LOOP('',(#7345,#7346,#7347,#7348));
#2150=EDGE_LOOP('',(#7349,#7350,#7351,#7352));
#2151=EDGE_LOOP('',(#7353,#7354,#7355,#7356));
#2152=EDGE_LOOP('',(#7357,#7358,#7359,#7360));
#2153=EDGE_LOOP('',(#7361,#7362,#7363,#7364));
#2154=EDGE_LOOP('',(#7365,#7366,#7367,#7368,#7369,#7370));
#2155=EDGE_LOOP('',(#7371,#7372,#7373,#7374,#7375,#7376));
#2156=EDGE_LOOP('',(#7377,#7378,#7379,#7380));
#2157=EDGE_LOOP('',(#7381,#7382,#7383,#7384));
#2158=EDGE_LOOP('',(#7385,#7386,#7387,#7388));
#2159=EDGE_LOOP('',(#7389,#7390,#7391,#7392));
#2160=EDGE_LOOP('',(#7393,#7394,#7395,#7396));
#2161=EDGE_LOOP('',(#7397));
#2162=EDGE_LOOP('',(#7398));
#2163=EDGE_LOOP('',(#7399,#7400,#7401,#7402));
#2164=EDGE_LOOP('',(#7403,#7404,#7405,#7406));
#2165=EDGE_LOOP('',(#7407,#7408,#7409,#7410));
#2166=EDGE_LOOP('',(#7411));
#2167=EDGE_LOOP('',(#7412));
#2168=EDGE_LOOP('',(#7413,#7414,#7415,#7416));
#2169=EDGE_LOOP('',(#7417,#7418,#7419,#7420));
#2170=EDGE_LOOP('',(#7421));
#2171=EDGE_LOOP('',(#7422));
#2172=EDGE_LOOP('',(#7423));
#2173=EDGE_LOOP('',(#7424));
#2174=EDGE_LOOP('',(#7425,#7426,#7427,#7428));
#2175=EDGE_LOOP('',(#7429,#7430,#7431,#7432));
#2176=EDGE_LOOP('',(#7433));
#2177=EDGE_LOOP('',(#7434));
#2178=EDGE_LOOP('',(#7435));
#2179=EDGE_LOOP('',(#7436));
#2180=EDGE_LOOP('',(#7437,#7438,#7439,#7440));
#2181=EDGE_LOOP('',(#7441));
#2182=EDGE_LOOP('',(#7442,#7443,#7444,#7445));
#2183=EDGE_LOOP('',(#7446));
#2184=EDGE_LOOP('',(#7447,#7448,#7449,#7450,#7451,#7452));
#2185=EDGE_LOOP('',(#7453,#7454,#7455,#7456));
#2186=EDGE_LOOP('',(#7457,#7458,#7459,#7460,#7461,#7462));
#2187=EDGE_LOOP('',(#7463,#7464,#7465,#7466));
#2188=EDGE_LOOP('',(#7467,#7468,#7469,#7470));
#2189=EDGE_LOOP('',(#7471,#7472,#7473,#7474,#7475,#7476));
#2190=EDGE_LOOP('',(#7477,#7478,#7479,#7480,#7481,#7482,#7483));
#2191=EDGE_LOOP('',(#7484,#7485,#7486,#7487,#7488,#7489,#7490));
#2192=EDGE_LOOP('',(#7491,#7492,#7493,#7494,#7495,#7496,#7497,#7498));
#2193=EDGE_LOOP('',(#7499));
#2194=EDGE_LOOP('',(#7500));
#2195=EDGE_LOOP('',(#7501,#7502));
#2196=EDGE_LOOP('',(#7503,#7504,#7505,#7506,#7507,#7508,#7509,#7510));
#2197=EDGE_LOOP('',(#7511,#7512,#7513));
#2198=EDGE_LOOP('',(#7514,#7515,#7516,#7517));
#2199=EDGE_LOOP('',(#7518,#7519,#7520,#7521));
#2200=EDGE_LOOP('',(#7522,#7523,#7524,#7525));
#2201=EDGE_LOOP('',(#7526));
#2202=EDGE_LOOP('',(#7527,#7528,#7529,#7530));
#2203=EDGE_LOOP('',(#7531,#7532,#7533,#7534));
#2204=EDGE_LOOP('',(#7535,#7536,#7537,#7538));
#2205=EDGE_LOOP('',(#7539,#7540,#7541,#7542));
#2206=EDGE_LOOP('',(#7543));
#2207=EDGE_LOOP('',(#7544,#7545,#7546,#7547));
#2208=EDGE_LOOP('',(#7548));
#2209=EDGE_LOOP('',(#7549));
#2210=EDGE_LOOP('',(#7550));
#2211=EDGE_LOOP('',(#7551,#7552,#7553,#7554));
#2212=EDGE_LOOP('',(#7555));
#2213=EDGE_LOOP('',(#7556,#7557,#7558,#7559));
#2214=EDGE_LOOP('',(#7560));
#2215=EDGE_LOOP('',(#7561,#7562,#7563,#7564));
#2216=EDGE_LOOP('',(#7565));
#2217=EDGE_LOOP('',(#7566));
#2218=EDGE_LOOP('',(#7567,#7568,#7569,#7570));
#2219=EDGE_LOOP('',(#7571,#7572,#7573,#7574));
#2220=EDGE_LOOP('',(#7575,#7576,#7577,#7578));
#2221=EDGE_LOOP('',(#7579,#7580,#7581,#7582));
#2222=EDGE_LOOP('',(#7583,#7584,#7585,#7586));
#2223=EDGE_LOOP('',(#7587,#7588,#7589,#7590));
#2224=EDGE_LOOP('',(#7591,#7592,#7593,#7594,#7595,#7596));
#2225=EDGE_LOOP('',(#7597));
#2226=EDGE_LOOP('',(#7598,#7599,#7600,#7601,#7602,#7603));
#2227=EDGE_LOOP('',(#7604,#7605,#7606,#7607));
#2228=EDGE_LOOP('',(#7608,#7609,#7610,#7611));
#2229=EDGE_LOOP('',(#7612,#7613,#7614,#7615));
#2230=EDGE_LOOP('',(#7616));
#2231=LINE('',#12373,#2861);
#2232=LINE('',#12379,#2862);
#2233=LINE('',#12385,#2863);
#2234=LINE('',#12391,#2864);
#2235=LINE('',#12397,#2865);
#2236=LINE('',#12403,#2866);
#2237=LINE('',#12409,#2867);
#2238=LINE('',#12415,#2868);
#2239=LINE('',#12421,#2869);
#2240=LINE('',#12427,#2870);
#2241=LINE('',#12433,#2871);
#2242=LINE('',#12439,#2872);
#2243=LINE('',#12444,#2873);
#2244=LINE('',#12446,#2874);
#2245=LINE('',#12448,#2875);
#2246=LINE('',#12449,#2876);
#2247=LINE('',#12452,#2877);
#2248=LINE('',#12454,#2878);
#2249=LINE('',#12455,#2879);
#2250=LINE('',#12458,#2880);
#2251=LINE('',#12460,#2881);
#2252=LINE('',#12461,#2882);
#2253=LINE('',#12463,#2883);
#2254=LINE('',#12464,#2884);
#2255=LINE('',#12472,#2885);
#2256=LINE('',#12478,#2886);
#2257=LINE('',#12484,#2887);
#2258=LINE('',#12490,#2888);
#2259=LINE('',#12495,#2889);
#2260=LINE('',#12497,#2890);
#2261=LINE('',#12499,#2891);
#2262=LINE('',#12500,#2892);
#2263=LINE('',#12503,#2893);
#2264=LINE('',#12505,#2894);
#2265=LINE('',#12506,#2895);
#2266=LINE('',#12509,#2896);
#2267=LINE('',#12511,#2897);
#2268=LINE('',#12512,#2898);
#2269=LINE('',#12514,#2899);
#2270=LINE('',#12515,#2900);
#2271=LINE('',#12522,#2901);
#2272=LINE('',#12524,#2902);
#2273=LINE('',#12526,#2903);
#2274=LINE('',#12527,#2904);
#2275=LINE('',#12530,#2905);
#2276=LINE('',#12532,#2906);
#2277=LINE('',#12533,#2907);
#2278=LINE('',#12536,#2908);
#2279=LINE('',#12538,#2909);
#2280=LINE('',#12539,#2910);
#2281=LINE('',#12541,#2911);
#2282=LINE('',#12542,#2912);
#2283=LINE('',#12549,#2913);
#2284=LINE('',#12551,#2914);
#2285=LINE('',#12553,#2915);
#2286=LINE('',#12554,#2916);
#2287=LINE('',#12557,#2917);
#2288=LINE('',#12559,#2918);
#2289=LINE('',#12560,#2919);
#2290=LINE('',#12563,#2920);
#2291=LINE('',#12565,#2921);
#2292=LINE('',#12566,#2922);
#2293=LINE('',#12568,#2923);
#2294=LINE('',#12569,#2924);
#2295=LINE('',#12577,#2925);
#2296=LINE('',#12583,#2926);
#2297=LINE('',#12590,#2927);
#2298=LINE('',#12597,#2928);
#2299=LINE('',#12604,#2929);
#2300=LINE('',#12611,#2930);
#2301=LINE('',#12617,#2931);
#2302=LINE('',#12623,#2932);
#2303=LINE('',#12629,#2933);
#2304=LINE('',#12635,#2934);
#2305=LINE('',#12641,#2935);
#2306=LINE('',#12647,#2936);
#2307=LINE('',#12653,#2937);
#2308=LINE('',#12659,#2938);
#2309=LINE('',#12667,#2939);
#2310=LINE('',#12672,#2940);
#2311=LINE('',#12677,#2941);
#2312=LINE('',#12681,#2942);
#2313=LINE('',#12685,#2943);
#2314=LINE('',#12687,#2944);
#2315=LINE('',#12689,#2945);
#2316=LINE('',#12691,#2946);
#2317=LINE('',#12693,#2947);
#2318=LINE('',#12695,#2948);
#2319=LINE('',#12697,#2949);
#2320=LINE('',#12700,#2950);
#2321=LINE('',#12703,#2951);
#2322=LINE('',#12704,#2952);
#2323=LINE('',#12708,#2953);
#2324=LINE('',#12710,#2954);
#2325=LINE('',#12712,#2955);
#2326=LINE('',#12713,#2956);
#2327=LINE('',#12716,#2957);
#2328=LINE('',#12717,#2958);
#2329=LINE('',#12718,#2959);
#2330=LINE('',#12722,#2960);
#2331=LINE('',#12723,#2961);
#2332=LINE('',#12724,#2962);
#2333=LINE('',#12727,#2963);
#2334=LINE('',#12728,#2964);
#2335=LINE('',#12731,#2965);
#2336=LINE('',#12732,#2966);
#2337=LINE('',#12734,#2967);
#2338=LINE('',#12737,#2968);
#2339=LINE('',#12738,#2969);
#2340=LINE('',#12741,#2970);
#2341=LINE('',#12743,#2971);
#2342=LINE('',#12746,#2972);
#2343=LINE('',#12747,#2973);
#2344=LINE('',#12749,#2974);
#2345=LINE('',#12751,#2975);
#2346=LINE('',#12752,#2976);
#2347=LINE('',#12756,#2977);
#2348=LINE('',#12758,#2978);
#2349=LINE('',#12766,#2979);
#2350=LINE('',#12772,#2980);
#2351=LINE('',#12778,#2981);
#2352=LINE('',#12784,#2982);
#2353=LINE('',#12790,#2983);
#2354=LINE('',#12797,#2984);
#2355=LINE('',#12803,#2985);
#2356=LINE('',#12812,#2986);
#2357=LINE('',#12818,#2987);
#2358=LINE('',#12824,#2988);
#2359=LINE('',#12830,#2989);
#2360=LINE('',#12836,#2990);
#2361=LINE('',#12844,#2991);
#2362=LINE('',#12849,#2992);
#2363=LINE('',#12858,#2993);
#2364=LINE('',#12867,#2994);
#2365=LINE('',#12876,#2995);
#2366=LINE('',#12885,#2996);
#2367=LINE('',#12893,#2997);
#2368=LINE('',#12897,#2998);
#2369=LINE('',#12901,#2999);
#2370=LINE('',#12905,#3000);
#2371=LINE('',#12910,#3001);
#2372=LINE('',#12918,#3002);
#2373=LINE('',#12923,#3003);
#2374=LINE('',#12931,#3004);
#2375=LINE('',#12933,#3005);
#2376=LINE('',#12935,#3006);
#2377=LINE('',#12936,#3007);
#2378=LINE('',#12939,#3008);
#2379=LINE('',#12941,#3009);
#2380=LINE('',#12942,#3010);
#2381=LINE('',#12945,#3011);
#2382=LINE('',#12947,#3012);
#2383=LINE('',#12948,#3013);
#2384=LINE('',#12950,#3014);
#2385=LINE('',#12951,#3015);
#2386=LINE('',#12959,#3016);
#2387=LINE('',#12966,#3017);
#2388=LINE('',#12972,#3018);
#2389=LINE('',#12974,#3019);
#2390=LINE('',#12976,#3020);
#2391=LINE('',#12977,#3021);
#2392=LINE('',#12980,#3022);
#2393=LINE('',#12982,#3023);
#2394=LINE('',#12983,#3024);
#2395=LINE('',#12986,#3025);
#2396=LINE('',#12988,#3026);
#2397=LINE('',#12989,#3027);
#2398=LINE('',#12991,#3028);
#2399=LINE('',#12992,#3029);
#2400=LINE('',#13000,#3030);
#2401=LINE('',#13007,#3031);
#2402=LINE('',#13013,#3032);
#2403=LINE('',#13015,#3033);
#2404=LINE('',#13017,#3034);
#2405=LINE('',#13018,#3035);
#2406=LINE('',#13021,#3036);
#2407=LINE('',#13023,#3037);
#2408=LINE('',#13024,#3038);
#2409=LINE('',#13027,#3039);
#2410=LINE('',#13029,#3040);
#2411=LINE('',#13030,#3041);
#2412=LINE('',#13032,#3042);
#2413=LINE('',#13033,#3043);
#2414=LINE('',#13041,#3044);
#2415=LINE('',#13052,#3045);
#2416=LINE('',#13056,#3046);
#2417=LINE('',#13063,#3047);
#2418=LINE('',#13065,#3048);
#2419=LINE('',#13067,#3049);
#2420=LINE('',#13068,#3050);
#2421=LINE('',#13071,#3051);
#2422=LINE('',#13073,#3052);
#2423=LINE('',#13074,#3053);
#2424=LINE('',#13077,#3054);
#2425=LINE('',#13079,#3055);
#2426=LINE('',#13080,#3056);
#2427=LINE('',#13083,#3057);
#2428=LINE('',#13085,#3058);
#2429=LINE('',#13086,#3059);
#2430=LINE('',#13089,#3060);
#2431=LINE('',#13091,#3061);
#2432=LINE('',#13092,#3062);
#2433=LINE('',#13095,#3063);
#2434=LINE('',#13097,#3064);
#2435=LINE('',#13098,#3065);
#2436=LINE('',#13101,#3066);
#2437=LINE('',#13103,#3067);
#2438=LINE('',#13104,#3068);
#2439=LINE('',#13107,#3069);
#2440=LINE('',#13109,#3070);
#2441=LINE('',#13110,#3071);
#2442=LINE('',#13113,#3072);
#2443=LINE('',#13115,#3073);
#2444=LINE('',#13116,#3074);
#2445=LINE('',#13120,#3075);
#2446=LINE('',#13122,#3076);
#2447=LINE('',#13124,#3077);
#2448=LINE('',#13125,#3078);
#2449=LINE('',#13128,#3079);
#2450=LINE('',#13130,#3080);
#2451=LINE('',#13131,#3081);
#2452=LINE('',#13134,#3082);
#2453=LINE('',#13136,#3083);
#2454=LINE('',#13137,#3084);
#2455=LINE('',#13140,#3085);
#2456=LINE('',#13142,#3086);
#2457=LINE('',#13143,#3087);
#2458=LINE('',#13146,#3088);
#2459=LINE('',#13148,#3089);
#2460=LINE('',#13149,#3090);
#2461=LINE('',#13152,#3091);
#2462=LINE('',#13154,#3092);
#2463=LINE('',#13155,#3093);
#2464=LINE('',#13158,#3094);
#2465=LINE('',#13160,#3095);
#2466=LINE('',#13161,#3096);
#2467=LINE('',#13164,#3097);
#2468=LINE('',#13166,#3098);
#2469=LINE('',#13167,#3099);
#2470=LINE('',#13170,#3100);
#2471=LINE('',#13172,#3101);
#2472=LINE('',#13173,#3102);
#2473=LINE('',#13177,#3103);
#2474=LINE('',#13179,#3104);
#2475=LINE('',#13181,#3105);
#2476=LINE('',#13182,#3106);
#2477=LINE('',#13185,#3107);
#2478=LINE('',#13187,#3108);
#2479=LINE('',#13188,#3109);
#2480=LINE('',#13191,#3110);
#2481=LINE('',#13193,#3111);
#2482=LINE('',#13194,#3112);
#2483=LINE('',#13197,#3113);
#2484=LINE('',#13199,#3114);
#2485=LINE('',#13200,#3115);
#2486=LINE('',#13203,#3116);
#2487=LINE('',#13205,#3117);
#2488=LINE('',#13206,#3118);
#2489=LINE('',#13209,#3119);
#2490=LINE('',#13211,#3120);
#2491=LINE('',#13212,#3121);
#2492=LINE('',#13215,#3122);
#2493=LINE('',#13217,#3123);
#2494=LINE('',#13218,#3124);
#2495=LINE('',#13221,#3125);
#2496=LINE('',#13223,#3126);
#2497=LINE('',#13224,#3127);
#2498=LINE('',#13227,#3128);
#2499=LINE('',#13229,#3129);
#2500=LINE('',#13230,#3130);
#2501=LINE('',#13234,#3131);
#2502=LINE('',#13236,#3132);
#2503=LINE('',#13238,#3133);
#2504=LINE('',#13239,#3134);
#2505=LINE('',#13242,#3135);
#2506=LINE('',#13244,#3136);
#2507=LINE('',#13245,#3137);
#2508=LINE('',#13248,#3138);
#2509=LINE('',#13250,#3139);
#2510=LINE('',#13251,#3140);
#2511=LINE('',#13254,#3141);
#2512=LINE('',#13256,#3142);
#2513=LINE('',#13257,#3143);
#2514=LINE('',#13260,#3144);
#2515=LINE('',#13262,#3145);
#2516=LINE('',#13263,#3146);
#2517=LINE('',#13266,#3147);
#2518=LINE('',#13268,#3148);
#2519=LINE('',#13269,#3149);
#2520=LINE('',#13272,#3150);
#2521=LINE('',#13274,#3151);
#2522=LINE('',#13275,#3152);
#2523=LINE('',#13278,#3153);
#2524=LINE('',#13280,#3154);
#2525=LINE('',#13281,#3155);
#2526=LINE('',#13284,#3156);
#2527=LINE('',#13286,#3157);
#2528=LINE('',#13287,#3158);
#2529=LINE('',#13292,#3159);
#2530=LINE('',#13296,#3160);
#2531=LINE('',#13298,#3161);
#2532=LINE('',#13299,#3162);
#2533=LINE('',#13302,#3163);
#2534=LINE('',#13304,#3164);
#2535=LINE('',#13305,#3165);
#2536=LINE('',#13307,#3166);
#2537=LINE('',#13308,#3167);
#2538=LINE('',#13311,#3168);
#2539=LINE('',#13313,#3169);
#2540=LINE('',#13314,#3170);
#2541=LINE('',#13316,#3171);
#2542=LINE('',#13317,#3172);
#2543=LINE('',#13320,#3173);
#2544=LINE('',#13322,#3174);
#2545=LINE('',#13323,#3175);
#2546=LINE('',#13325,#3176);
#2547=LINE('',#13326,#3177);
#2548=LINE('',#13328,#3178);
#2549=LINE('',#13329,#3179);
#2550=LINE('',#13336,#3180);
#2551=LINE('',#13338,#3181);
#2552=LINE('',#13340,#3182);
#2553=LINE('',#13341,#3183);
#2554=LINE('',#13344,#3184);
#2555=LINE('',#13346,#3185);
#2556=LINE('',#13347,#3186);
#2557=LINE('',#13350,#3187);
#2558=LINE('',#13352,#3188);
#2559=LINE('',#13353,#3189);
#2560=LINE('',#13358,#3190);
#2561=LINE('',#13360,#3191);
#2562=LINE('',#13362,#3192);
#2563=LINE('',#13364,#3193);
#2564=LINE('',#13366,#3194);
#2565=LINE('',#13368,#3195);
#2566=LINE('',#13369,#3196);
#2567=LINE('',#13372,#3197);
#2568=LINE('',#13373,#3198);
#2569=LINE('',#13376,#3199);
#2570=LINE('',#13377,#3200);
#2571=LINE('',#13380,#3201);
#2572=LINE('',#13382,#3202);
#2573=LINE('',#13384,#3203);
#2574=LINE('',#13386,#3204);
#2575=LINE('',#13387,#3205);
#2576=LINE('',#13389,#3206);
#2577=LINE('',#13392,#3207);
#2578=LINE('',#13395,#3208);
#2579=LINE('',#13399,#3209);
#2580=LINE('',#13406,#3210);
#2581=LINE('',#13408,#3211);
#2582=LINE('',#13410,#3212);
#2583=LINE('',#13417,#3213);
#2584=LINE('',#13421,#3214);
#2585=LINE('',#13428,#3215);
#2586=LINE('',#13435,#3216);
#2587=LINE('',#13437,#3217);
#2588=LINE('',#13439,#3218);
#2589=LINE('',#13440,#3219);
#2590=LINE('',#13443,#3220);
#2591=LINE('',#13445,#3221);
#2592=LINE('',#13446,#3222);
#2593=LINE('',#13449,#3223);
#2594=LINE('',#13451,#3224);
#2595=LINE('',#13452,#3225);
#2596=LINE('',#13455,#3226);
#2597=LINE('',#13457,#3227);
#2598=LINE('',#13458,#3228);
#2599=LINE('',#13461,#3229);
#2600=LINE('',#13463,#3230);
#2601=LINE('',#13464,#3231);
#2602=LINE('',#13466,#3232);
#2603=LINE('',#13467,#3233);
#2604=LINE('',#13479,#3234);
#2605=LINE('',#13483,#3235);
#2606=LINE('',#13487,#3236);
#2607=LINE('',#13494,#3237);
#2608=LINE('',#13496,#3238);
#2609=LINE('',#13511,#3239);
#2610=LINE('',#13517,#3240);
#2611=LINE('',#13521,#3241);
#2612=LINE('',#13527,#3242);
#2613=LINE('',#13532,#3243);
#2614=LINE('',#13547,#3244);
#2615=LINE('',#13556,#3245);
#2616=LINE('',#13560,#3246);
#2617=LINE('',#13564,#3247);
#2618=LINE('',#13567,#3248);
#2619=LINE('',#13720,#3249);
#2620=LINE('',#14016,#3250);
#2621=LINE('',#14058,#3251);
#2622=LINE('',#14063,#3252);
#2623=LINE('',#14072,#3253);
#2624=LINE('',#14077,#3254);
#2625=LINE('',#14090,#3255);
#2626=LINE('',#14092,#3256);
#2627=LINE('',#14093,#3257);
#2628=LINE('',#14096,#3258);
#2629=LINE('',#14098,#3259);
#2630=LINE('',#14099,#3260);
#2631=LINE('',#14104,#3261);
#2632=LINE('',#14105,#3262);
#2633=LINE('',#14107,#3263);
#2634=LINE('',#14108,#3264);
#2635=LINE('',#14118,#3265);
#2636=LINE('',#14125,#3266);
#2637=LINE('',#14132,#3267);
#2638=LINE('',#14139,#3268);
#2639=LINE('',#14146,#3269);
#2640=LINE('',#14151,#3270);
#2641=LINE('',#14158,#3271);
#2642=LINE('',#14161,#3272);
#2643=LINE('',#14164,#3273);
#2644=LINE('',#14166,#3274);
#2645=LINE('',#14167,#3275);
#2646=LINE('',#14173,#3276);
#2647=LINE('',#14175,#3277);
#2648=LINE('',#14176,#3278);
#2649=LINE('',#14185,#3279);
#2650=LINE('',#14190,#3280);
#2651=LINE('',#14197,#3281);
#2652=LINE('',#14199,#3282);
#2653=LINE('',#14201,#3283);
#2654=LINE('',#14202,#3284);
#2655=LINE('',#14205,#3285);
#2656=LINE('',#14207,#3286);
#2657=LINE('',#14208,#3287);
#2658=LINE('',#14211,#3288);
#2659=LINE('',#14213,#3289);
#2660=LINE('',#14214,#3290);
#2661=LINE('',#14217,#3291);
#2662=LINE('',#14219,#3292);
#2663=LINE('',#14220,#3293);
#2664=LINE('',#14223,#3294);
#2665=LINE('',#14225,#3295);
#2666=LINE('',#14226,#3296);
#2667=LINE('',#14228,#3297);
#2668=LINE('',#14229,#3298);
#2669=LINE('',#14239,#3299);
#2670=LINE('',#14248,#3300);
#2671=LINE('',#14252,#3301);
#2672=LINE('',#14256,#3302);
#2673=LINE('',#14263,#3303);
#2674=LINE('',#14267,#3304);
#2675=LINE('',#14269,#3305);
#2676=LINE('',#14276,#3306);
#2677=LINE('',#14281,#3307);
#2678=LINE('',#14285,#3308);
#2679=LINE('',#14289,#3309);
#2680=LINE('',#14295,#3310);
#2681=LINE('',#14299,#3311);
#2682=LINE('',#14302,#3312);
#2683=LINE('',#14307,#3313);
#2684=LINE('',#14308,#3314);
#2685=LINE('',#14311,#3315);
#2686=LINE('',#14314,#3316);
#2687=LINE('',#14317,#3317);
#2688=LINE('',#14320,#3318);
#2689=LINE('',#14323,#3319);
#2690=LINE('',#14324,#3320);
#2691=LINE('',#14327,#3321);
#2692=LINE('',#14330,#3322);
#2693=LINE('',#14337,#3323);
#2694=LINE('',#14344,#3324);
#2695=LINE('',#14347,#3325);
#2696=LINE('',#14352,#3326);
#2697=LINE('',#14360,#3327);
#2698=LINE('',#14366,#3328);
#2699=LINE('',#14374,#3329);
#2700=LINE('',#14395,#3330);
#2701=LINE('',#14450,#3331);
#2702=LINE('',#14455,#3332);
#2703=LINE('',#14461,#3333);
#2704=LINE('',#14470,#3334);
#2705=LINE('',#14477,#3335);
#2706=LINE('',#14491,#3336);
#2707=LINE('',#14494,#3337);
#2708=LINE('',#14499,#3338);
#2709=LINE('',#14507,#3339);
#2710=LINE('',#14513,#3340);
#2711=LINE('',#14522,#3341);
#2712=LINE('',#14528,#3342);
#2713=LINE('',#14537,#3343);
#2714=LINE('',#14543,#3344);
#2715=LINE('',#14552,#3345);
#2716=LINE('',#14558,#3346);
#2717=LINE('',#14569,#3347);
#2718=LINE('',#14571,#3348);
#2719=LINE('',#14573,#3349);
#2720=LINE('',#14574,#3350);
#2721=LINE('',#14577,#3351);
#2722=LINE('',#14579,#3352);
#2723=LINE('',#14580,#3353);
#2724=LINE('',#14583,#3354);
#2725=LINE('',#14585,#3355);
#2726=LINE('',#14586,#3356);
#2727=LINE('',#14589,#3357);
#2728=LINE('',#14591,#3358);
#2729=LINE('',#14592,#3359);
#2730=LINE('',#14595,#3360);
#2731=LINE('',#14597,#3361);
#2732=LINE('',#14598,#3362);
#2733=LINE('',#14600,#3363);
#2734=LINE('',#14601,#3364);
#2735=LINE('',#14609,#3365);
#2736=LINE('',#14611,#3366);
#2737=LINE('',#14616,#3367);
#2738=LINE('',#14618,#3368);
#2739=LINE('',#14620,#3369);
#2740=LINE('',#14621,#3370);
#2741=LINE('',#14624,#3371);
#2742=LINE('',#14626,#3372);
#2743=LINE('',#14627,#3373);
#2744=LINE('',#14630,#3374);
#2745=LINE('',#14632,#3375);
#2746=LINE('',#14633,#3376);
#2747=LINE('',#14636,#3377);
#2748=LINE('',#14638,#3378);
#2749=LINE('',#14639,#3379);
#2750=LINE('',#14642,#3380);
#2751=LINE('',#14644,#3381);
#2752=LINE('',#14645,#3382);
#2753=LINE('',#14647,#3383);
#2754=LINE('',#14648,#3384);
#2755=LINE('',#14660,#3385);
#2756=LINE('',#14664,#3386);
#2757=LINE('',#14668,#3387);
#2758=LINE('',#14675,#3388);
#2759=LINE('',#14677,#3389);
#2760=LINE('',#14685,#3390);
#2761=LINE('',#14689,#3391);
#2762=LINE('',#14693,#3392);
#2763=LINE('',#14700,#3393);
#2764=LINE('',#14704,#3394);
#2765=LINE('',#14708,#3395);
#2766=LINE('',#14713,#3396);
#2767=LINE('',#14715,#3397);
#2768=LINE('',#14717,#3398);
#2769=LINE('',#14718,#3399);
#2770=LINE('',#14721,#3400);
#2771=LINE('',#14723,#3401);
#2772=LINE('',#14724,#3402);
#2773=LINE('',#14727,#3403);
#2774=LINE('',#14729,#3404);
#2775=LINE('',#14730,#3405);
#2776=LINE('',#14733,#3406);
#2777=LINE('',#14735,#3407);
#2778=LINE('',#14736,#3408);
#2779=LINE('',#14739,#3409);
#2780=LINE('',#14741,#3410);
#2781=LINE('',#14742,#3411);
#2782=LINE('',#14744,#3412);
#2783=LINE('',#14745,#3413);
#2784=LINE('',#14822,#3414);
#2785=LINE('',#14828,#3415);
#2786=LINE('',#14833,#3416);
#2787=LINE('',#14837,#3417);
#2788=LINE('',#14841,#3418);
#2789=LINE('',#14843,#3419);
#2790=LINE('',#14844,#3420);
#2791=LINE('',#14847,#3421);
#2792=LINE('',#14851,#3422);
#2793=LINE('',#14852,#3423);
#2794=LINE('',#14861,#3424);
#2795=LINE('',#14867,#3425);
#2796=LINE('',#14876,#3426);
#2797=LINE('',#14882,#3427);
#2798=LINE('',#14895,#3428);
#2799=LINE('',#14901,#3429);
#2800=LINE('',#14903,#3430);
#2801=LINE('',#14905,#3431);
#2802=LINE('',#14906,#3432);
#2803=LINE('',#14909,#3433);
#2804=LINE('',#14911,#3434);
#2805=LINE('',#14913,#3435);
#2806=LINE('',#14915,#3436);
#2807=LINE('',#14916,#3437);
#2808=LINE('',#14919,#3438);
#2809=LINE('',#14923,#3439);
#2810=LINE('',#14925,#3440);
#2811=LINE('',#14927,#3441);
#2812=LINE('',#14928,#3442);
#2813=LINE('',#14932,#3443);
#2814=LINE('',#14933,#3444);
#2815=LINE('',#14934,#3445);
#2816=LINE('',#14937,#3446);
#2817=LINE('',#14939,#3447);
#2818=LINE('',#14940,#3448);
#2819=LINE('',#14946,#3449);
#2820=LINE('',#14954,#3450);
#2821=LINE('',#14961,#3451);
#2822=LINE('',#14978,#3452);
#2823=LINE('',#14993,#3453);
#2824=LINE('',#14998,#3454);
#2825=LINE('',#15003,#3455);
#2826=LINE('',#15005,#3456);
#2827=LINE('',#15007,#3457);
#2828=LINE('',#15008,#3458);
#2829=LINE('',#15012,#3459);
#2830=LINE('',#15013,#3460);
#2831=LINE('',#15014,#3461);
#2832=LINE('',#15017,#3462);
#2833=LINE('',#15018,#3463);
#2834=LINE('',#15021,#3464);
#2835=LINE('',#15022,#3465);
#2836=LINE('',#15024,#3466);
#2837=LINE('',#15034,#3467);
#2838=LINE('',#15040,#3468);
#2839=LINE('',#15047,#3469);
#2840=LINE('',#15055,#3470);
#2841=LINE('',#15057,#3471);
#2842=LINE('',#15059,#3472);
#2843=LINE('',#15060,#3473);
#2844=LINE('',#15063,#3474);
#2845=LINE('',#15065,#3475);
#2846=LINE('',#15066,#3476);
#2847=LINE('',#15069,#3477);
#2848=LINE('',#15071,#3478);
#2849=LINE('',#15072,#3479);
#2850=LINE('',#15075,#3480);
#2851=LINE('',#15077,#3481);
#2852=LINE('',#15078,#3482);
#2853=LINE('',#15081,#3483);
#2854=LINE('',#15083,#3484);
#2855=LINE('',#15084,#3485);
#2856=LINE('',#15086,#3486);
#2857=LINE('',#15087,#3487);
#2858=LINE('',#15095,#3488);
#2859=LINE('',#15099,#3489);
#2860=LINE('',#15103,#3490);
#2861=VECTOR('',#9764,0.225);
#2862=VECTOR('',#9771,0.225);
#2863=VECTOR('',#9778,0.225);
#2864=VECTOR('',#9785,0.225);
#2865=VECTOR('',#9792,0.21);
#2866=VECTOR('',#9799,0.210000000000001);
#2867=VECTOR('',#9806,0.210000000000001);
#2868=VECTOR('',#9813,0.21);
#2869=VECTOR('',#9820,0.275);
#2870=VECTOR('',#9827,0.275);
#2871=VECTOR('',#9834,0.275);
#2872=VECTOR('',#9841,0.275);
#2873=VECTOR('',#9846,1.);
#2874=VECTOR('',#9847,1.);
#2875=VECTOR('',#9848,1.);
#2876=VECTOR('',#9849,1.);
#2877=VECTOR('',#9852,1.);
#2878=VECTOR('',#9853,1.);
#2879=VECTOR('',#9854,1.);
#2880=VECTOR('',#9857,1.);
#2881=VECTOR('',#9858,1.);
#2882=VECTOR('',#9859,1.);
#2883=VECTOR('',#9862,1.);
#2884=VECTOR('',#9863,1.);
#2885=VECTOR('',#9874,0.275);
#2886=VECTOR('',#9881,0.275);
#2887=VECTOR('',#9888,0.275);
#2888=VECTOR('',#9895,0.275);
#2889=VECTOR('',#9900,1.);
#2890=VECTOR('',#9901,1.);
#2891=VECTOR('',#9902,1.);
#2892=VECTOR('',#9903,1.);
#2893=VECTOR('',#9906,1.);
#2894=VECTOR('',#9907,1.);
#2895=VECTOR('',#9908,1.);
#2896=VECTOR('',#9911,1.);
#2897=VECTOR('',#9912,1.);
#2898=VECTOR('',#9913,1.);
#2899=VECTOR('',#9916,1.);
#2900=VECTOR('',#9917,1.);
#2901=VECTOR('',#9926,1.);
#2902=VECTOR('',#9927,1.);
#2903=VECTOR('',#9928,1.);
#2904=VECTOR('',#9929,1.);
#2905=VECTOR('',#9932,1.);
#2906=VECTOR('',#9933,1.);
#2907=VECTOR('',#9934,1.);
#2908=VECTOR('',#9937,1.);
#2909=VECTOR('',#9938,1.);
#2910=VECTOR('',#9939,1.);
#2911=VECTOR('',#9942,1.);
#2912=VECTOR('',#9943,1.);
#2913=VECTOR('',#9952,1.);
#2914=VECTOR('',#9953,1.);
#2915=VECTOR('',#9954,1.);
#2916=VECTOR('',#9955,1.);
#2917=VECTOR('',#9958,1.);
#2918=VECTOR('',#9959,1.);
#2919=VECTOR('',#9960,1.);
#2920=VECTOR('',#9963,1.);
#2921=VECTOR('',#9964,1.);
#2922=VECTOR('',#9965,1.);
#2923=VECTOR('',#9968,1.);
#2924=VECTOR('',#9969,1.);
#2925=VECTOR('',#9980,0.225);
#2926=VECTOR('',#9987,0.165);
#2927=VECTOR('',#9996,0.165);
#2928=VECTOR('',#10005,0.165);
#2929=VECTOR('',#10014,0.165);
#2930=VECTOR('',#10023,0.165);
#2931=VECTOR('',#10030,0.165);
#2932=VECTOR('',#10037,0.165);
#2933=VECTOR('',#10044,0.165);
#2934=VECTOR('',#10051,0.275);
#2935=VECTOR('',#10058,0.275);
#2936=VECTOR('',#10065,0.275);
#2937=VECTOR('',#10072,0.275);
#2938=VECTOR('',#10079,1.05);
#2939=VECTOR('',#10090,0.625);
#2940=VECTOR('',#10095,1.5);
#2941=VECTOR('',#10100,1.);
#2942=VECTOR('',#10103,1.);
#2943=VECTOR('',#10108,1.);
#2944=VECTOR('',#10109,1.);
#2945=VECTOR('',#10110,1.);
#2946=VECTOR('',#10111,1.);
#2947=VECTOR('',#10112,1.);
#2948=VECTOR('',#10113,1.);
#2949=VECTOR('',#10114,1.);
#2950=VECTOR('',#10117,1.);
#2951=VECTOR('',#10120,1.);
#2952=VECTOR('',#10121,1.);
#2953=VECTOR('',#10124,1.);
#2954=VECTOR('',#10125,1.);
#2955=VECTOR('',#10126,1.);
#2956=VECTOR('',#10127,1.);
#2957=VECTOR('',#10128,1.);
#2958=VECTOR('',#10129,1.);
#2959=VECTOR('',#10130,1.);
#2960=VECTOR('',#10133,1.);
#2961=VECTOR('',#10134,1.);
#2962=VECTOR('',#10135,1.);
#2963=VECTOR('',#10138,1.);
#2964=VECTOR('',#10139,1.);
#2965=VECTOR('',#10142,1.);
#2966=VECTOR('',#10143,1.);
#2967=VECTOR('',#10146,1.);
#2968=VECTOR('',#10149,1.);
#2969=VECTOR('',#10150,1.);
#2970=VECTOR('',#10153,1.);
#2971=VECTOR('',#10154,1.);
#2972=VECTOR('',#10159,1.);
#2973=VECTOR('',#10160,1.);
#2974=VECTOR('',#10161,1.);
#2975=VECTOR('',#10162,1.);
#2976=VECTOR('',#10163,1.);
#2977=VECTOR('',#10170,1.);
#2978=VECTOR('',#10173,1.);
#2979=VECTOR('',#10184,0.225);
#2980=VECTOR('',#10191,0.225);
#2981=VECTOR('',#10198,0.225);
#2982=VECTOR('',#10205,0.225);
#2983=VECTOR('',#10212,1.49);
#2984=VECTOR('',#10221,0.71);
#2985=VECTOR('',#10228,2.2);
#2986=VECTOR('',#10241,0.225);
#2987=VECTOR('',#10248,0.225);
#2988=VECTOR('',#10255,0.225);
#2989=VECTOR('',#10262,0.225);
#2990=VECTOR('',#10269,1.49);
#2991=VECTOR('',#10280,0.71);
#2992=VECTOR('',#10285,2.2);
#2993=VECTOR('',#10298,0.375);
#2994=VECTOR('',#10309,0.375);
#2995=VECTOR('',#10320,0.375);
#2996=VECTOR('',#10331,0.375);
#2997=VECTOR('',#10342,0.225);
#2998=VECTOR('',#10347,0.225);
#2999=VECTOR('',#10352,0.225);
#3000=VECTOR('',#10357,0.225);
#3001=VECTOR('',#10362,1.04);
#3002=VECTOR('',#10373,0.625);
#3003=VECTOR('',#10378,2.);
#3004=VECTOR('',#10389,1.);
#3005=VECTOR('',#10390,1.);
#3006=VECTOR('',#10391,1.);
#3007=VECTOR('',#10392,1.);
#3008=VECTOR('',#10395,1.);
#3009=VECTOR('',#10396,1.);
#3010=VECTOR('',#10397,1.);
#3011=VECTOR('',#10400,1.);
#3012=VECTOR('',#10401,1.);
#3013=VECTOR('',#10402,1.);
#3014=VECTOR('',#10405,1.);
#3015=VECTOR('',#10406,1.);
#3016=VECTOR('',#10417,0.165);
#3017=VECTOR('',#10426,0.165);
#3018=VECTOR('',#10433,1.);
#3019=VECTOR('',#10434,1.);
#3020=VECTOR('',#10435,1.);
#3021=VECTOR('',#10436,1.);
#3022=VECTOR('',#10439,1.);
#3023=VECTOR('',#10440,1.);
#3024=VECTOR('',#10441,1.);
#3025=VECTOR('',#10444,1.);
#3026=VECTOR('',#10445,1.);
#3027=VECTOR('',#10446,1.);
#3028=VECTOR('',#10449,1.);
#3029=VECTOR('',#10450,1.);
#3030=VECTOR('',#10461,0.165);
#3031=VECTOR('',#10470,0.165);
#3032=VECTOR('',#10477,1.);
#3033=VECTOR('',#10478,1.);
#3034=VECTOR('',#10479,1.);
#3035=VECTOR('',#10480,1.);
#3036=VECTOR('',#10483,1.);
#3037=VECTOR('',#10484,1.);
#3038=VECTOR('',#10485,1.);
#3039=VECTOR('',#10488,1.);
#3040=VECTOR('',#10489,1.);
#3041=VECTOR('',#10490,1.);
#3042=VECTOR('',#10493,1.);
#3043=VECTOR('',#10494,1.);
#3044=VECTOR('',#10505,0.165);
#3045=VECTOR('',#10520,0.5);
#3046=VECTOR('',#10525,0.3);
#3047=VECTOR('',#10534,1.);
#3048=VECTOR('',#10535,1.);
#3049=VECTOR('',#10536,1.);
#3050=VECTOR('',#10537,1.);
#3051=VECTOR('',#10540,1.);
#3052=VECTOR('',#10541,1.);
#3053=VECTOR('',#10542,1.);
#3054=VECTOR('',#10545,1.);
#3055=VECTOR('',#10546,1.);
#3056=VECTOR('',#10547,1.);
#3057=VECTOR('',#10550,1.);
#3058=VECTOR('',#10551,1.);
#3059=VECTOR('',#10552,1.);
#3060=VECTOR('',#10555,1.);
#3061=VECTOR('',#10556,1.);
#3062=VECTOR('',#10557,1.);
#3063=VECTOR('',#10560,1.);
#3064=VECTOR('',#10561,1.);
#3065=VECTOR('',#10562,1.);
#3066=VECTOR('',#10565,1.);
#3067=VECTOR('',#10566,1.);
#3068=VECTOR('',#10567,1.);
#3069=VECTOR('',#10570,1.);
#3070=VECTOR('',#10571,1.);
#3071=VECTOR('',#10572,1.);
#3072=VECTOR('',#10575,1.);
#3073=VECTOR('',#10576,1.);
#3074=VECTOR('',#10577,1.);
#3075=VECTOR('',#10580,1.);
#3076=VECTOR('',#10581,1.);
#3077=VECTOR('',#10582,1.);
#3078=VECTOR('',#10583,1.);
#3079=VECTOR('',#10586,1.);
#3080=VECTOR('',#10587,1.);
#3081=VECTOR('',#10588,1.);
#3082=VECTOR('',#10591,1.);
#3083=VECTOR('',#10592,1.);
#3084=VECTOR('',#10593,1.);
#3085=VECTOR('',#10596,1.);
#3086=VECTOR('',#10597,1.);
#3087=VECTOR('',#10598,1.);
#3088=VECTOR('',#10601,1.);
#3089=VECTOR('',#10602,1.);
#3090=VECTOR('',#10603,1.);
#3091=VECTOR('',#10606,1.);
#3092=VECTOR('',#10607,1.);
#3093=VECTOR('',#10608,1.);
#3094=VECTOR('',#10611,1.);
#3095=VECTOR('',#10612,1.);
#3096=VECTOR('',#10613,1.);
#3097=VECTOR('',#10616,1.);
#3098=VECTOR('',#10617,1.);
#3099=VECTOR('',#10618,1.);
#3100=VECTOR('',#10621,1.);
#3101=VECTOR('',#10622,1.);
#3102=VECTOR('',#10623,1.);
#3103=VECTOR('',#10626,1.);
#3104=VECTOR('',#10627,1.);
#3105=VECTOR('',#10628,1.);
#3106=VECTOR('',#10629,1.);
#3107=VECTOR('',#10632,1.);
#3108=VECTOR('',#10633,1.);
#3109=VECTOR('',#10634,1.);
#3110=VECTOR('',#10637,1.);
#3111=VECTOR('',#10638,1.);
#3112=VECTOR('',#10639,1.);
#3113=VECTOR('',#10642,1.);
#3114=VECTOR('',#10643,1.);
#3115=VECTOR('',#10644,1.);
#3116=VECTOR('',#10647,1.);
#3117=VECTOR('',#10648,1.);
#3118=VECTOR('',#10649,1.);
#3119=VECTOR('',#10652,1.);
#3120=VECTOR('',#10653,1.);
#3121=VECTOR('',#10654,1.);
#3122=VECTOR('',#10657,1.);
#3123=VECTOR('',#10658,1.);
#3124=VECTOR('',#10659,1.);
#3125=VECTOR('',#10662,1.);
#3126=VECTOR('',#10663,1.);
#3127=VECTOR('',#10664,1.);
#3128=VECTOR('',#10667,1.);
#3129=VECTOR('',#10668,1.);
#3130=VECTOR('',#10669,1.);
#3131=VECTOR('',#10672,1.);
#3132=VECTOR('',#10673,1.);
#3133=VECTOR('',#10674,1.);
#3134=VECTOR('',#10675,1.);
#3135=VECTOR('',#10678,1.);
#3136=VECTOR('',#10679,1.);
#3137=VECTOR('',#10680,1.);
#3138=VECTOR('',#10683,1.);
#3139=VECTOR('',#10684,1.);
#3140=VECTOR('',#10685,1.);
#3141=VECTOR('',#10688,1.);
#3142=VECTOR('',#10689,1.);
#3143=VECTOR('',#10690,1.);
#3144=VECTOR('',#10693,1.);
#3145=VECTOR('',#10694,1.);
#3146=VECTOR('',#10695,1.);
#3147=VECTOR('',#10698,1.);
#3148=VECTOR('',#10699,1.);
#3149=VECTOR('',#10700,1.);
#3150=VECTOR('',#10703,1.);
#3151=VECTOR('',#10704,1.);
#3152=VECTOR('',#10705,1.);
#3153=VECTOR('',#10708,1.);
#3154=VECTOR('',#10709,1.);
#3155=VECTOR('',#10710,1.);
#3156=VECTOR('',#10713,1.);
#3157=VECTOR('',#10714,1.);
#3158=VECTOR('',#10715,1.);
#3159=VECTOR('',#10720,0.21);
#3160=VECTOR('',#10725,1.);
#3161=VECTOR('',#10726,1.);
#3162=VECTOR('',#10727,1.);
#3163=VECTOR('',#10730,1.);
#3164=VECTOR('',#10731,1.);
#3165=VECTOR('',#10732,1.);
#3166=VECTOR('',#10735,1.);
#3167=VECTOR('',#10736,1.);
#3168=VECTOR('',#10739,1.);
#3169=VECTOR('',#10740,1.);
#3170=VECTOR('',#10741,1.);
#3171=VECTOR('',#10744,1.);
#3172=VECTOR('',#10745,1.);
#3173=VECTOR('',#10748,1.);
#3174=VECTOR('',#10749,1.);
#3175=VECTOR('',#10750,1.);
#3176=VECTOR('',#10753,1.);
#3177=VECTOR('',#10754,1.);
#3178=VECTOR('',#10757,1.);
#3179=VECTOR('',#10758,1.);
#3180=VECTOR('',#10767,1.);
#3181=VECTOR('',#10768,1.);
#3182=VECTOR('',#10769,1.);
#3183=VECTOR('',#10770,1.);
#3184=VECTOR('',#10773,1.);
#3185=VECTOR('',#10774,1.);
#3186=VECTOR('',#10775,1.);
#3187=VECTOR('',#10778,1.);
#3188=VECTOR('',#10779,1.);
#3189=VECTOR('',#10780,1.);
#3190=VECTOR('',#10785,1.);
#3191=VECTOR('',#10786,1.);
#3192=VECTOR('',#10787,1.);
#3193=VECTOR('',#10788,1.);
#3194=VECTOR('',#10789,1.);
#3195=VECTOR('',#10790,1.);
#3196=VECTOR('',#10791,1.);
#3197=VECTOR('',#10794,1.);
#3198=VECTOR('',#10795,1.);
#3199=VECTOR('',#10798,1.);
#3200=VECTOR('',#10799,1.);
#3201=VECTOR('',#10802,1.);
#3202=VECTOR('',#10803,1.);
#3203=VECTOR('',#10804,1.);
#3204=VECTOR('',#10805,1.);
#3205=VECTOR('',#10806,1.);
#3206=VECTOR('',#10809,1.);
#3207=VECTOR('',#10812,1.);
#3208=VECTOR('',#10815,1.);
#3209=VECTOR('',#10820,0.21);
#3210=VECTOR('',#10829,1.);
#3211=VECTOR('',#10832,1.);
#3212=VECTOR('',#10835,1.);
#3213=VECTOR('',#10844,0.275);
#3214=VECTOR('',#10849,0.265);
#3215=VECTOR('',#10858,0.5);
#3216=VECTOR('',#10867,1.);
#3217=VECTOR('',#10868,1.);
#3218=VECTOR('',#10869,1.);
#3219=VECTOR('',#10870,1.);
#3220=VECTOR('',#10873,1.);
#3221=VECTOR('',#10874,1.);
#3222=VECTOR('',#10875,1.);
#3223=VECTOR('',#10878,1.);
#3224=VECTOR('',#10879,1.);
#3225=VECTOR('',#10880,1.);
#3226=VECTOR('',#10883,1.);
#3227=VECTOR('',#10884,1.);
#3228=VECTOR('',#10885,1.);
#3229=VECTOR('',#10888,1.);
#3230=VECTOR('',#10889,1.);
#3231=VECTOR('',#10890,1.);
#3232=VECTOR('',#10893,1.);
#3233=VECTOR('',#10894,1.);
#3234=VECTOR('',#10911,0.4);
#3235=VECTOR('',#10916,0.425);
#3236=VECTOR('',#10921,0.41);
#3237=VECTOR('',#10930,0.26);
#3238=VECTOR('',#10933,0.25);
#3239=VECTOR('',#10952,0.976185);
#3240=VECTOR('',#10959,0.5);
#3241=VECTOR('',#10964,0.53);
#3242=VECTOR('',#10973,0.976185);
#3243=VECTOR('',#10980,0.53);
#3244=VECTOR('',#10999,1.023815);
#3245=VECTOR('',#11010,1.47);
#3246=VECTOR('',#11015,1.5);
#3247=VECTOR('',#11020,1.47);
#3248=VECTOR('',#11025,1.023815);
#3249=VECTOR('',#11076,1.019052);
#3250=VECTOR('',#11153,0.980948);
#3251=VECTOR('',#11182,1.013815);
#3252=VECTOR('',#11189,0.991185);
#3253=VECTOR('',#11200,1.013815);
#3254=VECTOR('',#11207,0.991185);
#3255=VECTOR('',#11226,1.);
#3256=VECTOR('',#11227,1.);
#3257=VECTOR('',#11228,1.);
#3258=VECTOR('',#11231,1.);
#3259=VECTOR('',#11232,1.);
#3260=VECTOR('',#11233,1.);
#3261=VECTOR('',#11238,1.);
#3262=VECTOR('',#11239,1.);
#3263=VECTOR('',#11242,1.);
#3264=VECTOR('',#11243,1.);
#3265=VECTOR('',#11256,1.05);
#3266=VECTOR('',#11265,1.);
#3267=VECTOR('',#11274,1.05);
#3268=VECTOR('',#11283,1.);
#3269=VECTOR('',#11292,1.05);
#3270=VECTOR('',#11299,0.9);
#3271=VECTOR('',#11306,1.);
#3272=VECTOR('',#11309,1.);
#3273=VECTOR('',#11312,1.);
#3274=VECTOR('',#11313,1.);
#3275=VECTOR('',#11314,1.);
#3276=VECTOR('',#11321,1.);
#3277=VECTOR('',#11324,1.);
#3278=VECTOR('',#11325,1.);
#3279=VECTOR('',#11336,0.895);
#3280=VECTOR('',#11343,0.605);
#3281=VECTOR('',#11352,1.);
#3282=VECTOR('',#11353,1.);
#3283=VECTOR('',#11354,1.);
#3284=VECTOR('',#11355,1.);
#3285=VECTOR('',#11358,1.);
#3286=VECTOR('',#11359,1.);
#3287=VECTOR('',#11360,1.);
#3288=VECTOR('',#11363,1.);
#3289=VECTOR('',#11364,1.);
#3290=VECTOR('',#11365,1.);
#3291=VECTOR('',#11368,1.);
#3292=VECTOR('',#11369,1.);
#3293=VECTOR('',#11370,1.);
#3294=VECTOR('',#11373,1.);
#3295=VECTOR('',#11374,1.);
#3296=VECTOR('',#11375,1.);
#3297=VECTOR('',#11378,1.);
#3298=VECTOR('',#11379,1.);
#3299=VECTOR('',#11392,0.2);
#3300=VECTOR('',#11405,0.325);
#3301=VECTOR('',#11410,0.35);
#3302=VECTOR('',#11415,0.335);
#3303=VECTOR('',#11424,0.21);
#3304=VECTOR('',#11429,0.2);
#3305=VECTOR('',#11432,0.18);
#3306=VECTOR('',#11441,0.305);
#3307=VECTOR('',#11446,1.);
#3308=VECTOR('',#11449,1.);
#3309=VECTOR('',#11454,1.);
#3310=VECTOR('',#11459,1.);
#3311=VECTOR('',#11462,1.);
#3312=VECTOR('',#11465,1.);
#3313=VECTOR('',#11470,1.);
#3314=VECTOR('',#11471,1.);
#3315=VECTOR('',#11474,1.);
#3316=VECTOR('',#11479,1.);
#3317=VECTOR('',#11482,1.);
#3318=VECTOR('',#11485,1.);
#3319=VECTOR('',#11488,1.);
#3320=VECTOR('',#11489,1.);
#3321=VECTOR('',#11492,1.);
#3322=VECTOR('',#11497,1.);
#3323=VECTOR('',#11506,1.);
#3324=VECTOR('',#11515,0.7);
#3325=VECTOR('',#11518,0.5);
#3326=VECTOR('',#11525,0.5);
#3327=VECTOR('',#11536,0.505);
#3328=VECTOR('',#11543,0.7);
#3329=VECTOR('',#11554,1.);
#3330=VECTOR('',#11561,0.164999999999999);
#3331=VECTOR('',#11566,1.);
#3332=VECTOR('',#11571,0.505);
#3333=VECTOR('',#11578,0.9);
#3334=VECTOR('',#11591,0.165);
#3335=VECTOR('',#11600,0.165);
#3336=VECTOR('',#11619,0.7);
#3337=VECTOR('',#11622,0.3);
#3338=VECTOR('',#11629,0.3);
#3339=VECTOR('',#11640,0.305);
#3340=VECTOR('',#11647,0.5);
#3341=VECTOR('',#11660,0.305);
#3342=VECTOR('',#11667,0.5);
#3343=VECTOR('',#11680,0.225);
#3344=VECTOR('',#11687,0.5);
#3345=VECTOR('',#11700,0.225);
#3346=VECTOR('',#11707,0.5);
#3347=VECTOR('',#11722,1.);
#3348=VECTOR('',#11723,1.);
#3349=VECTOR('',#11724,1.);
#3350=VECTOR('',#11725,1.);
#3351=VECTOR('',#11728,1.);
#3352=VECTOR('',#11729,1.);
#3353=VECTOR('',#11730,1.);
#3354=VECTOR('',#11733,1.);
#3355=VECTOR('',#11734,1.);
#3356=VECTOR('',#11735,1.);
#3357=VECTOR('',#11738,1.);
#3358=VECTOR('',#11739,1.);
#3359=VECTOR('',#11740,1.);
#3360=VECTOR('',#11743,1.);
#3361=VECTOR('',#11744,1.);
#3362=VECTOR('',#11745,1.);
#3363=VECTOR('',#11748,1.);
#3364=VECTOR('',#11749,1.);
#3365=VECTOR('',#11760,0.185);
#3366=VECTOR('',#11763,0.2);
#3367=VECTOR('',#11768,1.);
#3368=VECTOR('',#11769,1.);
#3369=VECTOR('',#11770,1.);
#3370=VECTOR('',#11771,1.);
#3371=VECTOR('',#11774,1.);
#3372=VECTOR('',#11775,1.);
#3373=VECTOR('',#11776,1.);
#3374=VECTOR('',#11779,1.);
#3375=VECTOR('',#11780,1.);
#3376=VECTOR('',#11781,1.);
#3377=VECTOR('',#11784,1.);
#3378=VECTOR('',#11785,1.);
#3379=VECTOR('',#11786,1.);
#3380=VECTOR('',#11789,1.);
#3381=VECTOR('',#11790,1.);
#3382=VECTOR('',#11791,1.);
#3383=VECTOR('',#11794,1.);
#3384=VECTOR('',#11795,1.);
#3385=VECTOR('',#11812,0.325);
#3386=VECTOR('',#11817,0.35);
#3387=VECTOR('',#11822,0.335);
#3388=VECTOR('',#11831,0.21);
#3389=VECTOR('',#11834,0.2);
#3390=VECTOR('',#11845,0.325);
#3391=VECTOR('',#11850,0.35);
#3392=VECTOR('',#11855,0.335);
#3393=VECTOR('',#11864,0.21);
#3394=VECTOR('',#11869,0.2);
#3395=VECTOR('',#11874,0.18);
#3396=VECTOR('',#11879,1.);
#3397=VECTOR('',#11880,1.);
#3398=VECTOR('',#11881,1.);
#3399=VECTOR('',#11882,1.);
#3400=VECTOR('',#11885,1.);
#3401=VECTOR('',#11886,1.);
#3402=VECTOR('',#11887,1.);
#3403=VECTOR('',#11890,1.);
#3404=VECTOR('',#11891,1.);
#3405=VECTOR('',#11892,1.);
#3406=VECTOR('',#11895,1.);
#3407=VECTOR('',#11896,1.);
#3408=VECTOR('',#11897,1.);
#3409=VECTOR('',#11900,1.);
#3410=VECTOR('',#11901,1.);
#3411=VECTOR('',#11902,1.);
#3412=VECTOR('',#11905,1.);
#3413=VECTOR('',#11906,1.);
#3414=VECTOR('',#12055,0.5);
#3415=VECTOR('',#12062,0.5);
#3416=VECTOR('',#12067,1.);
#3417=VECTOR('',#12070,1.);
#3418=VECTOR('',#12075,1.);
#3419=VECTOR('',#12076,1.);
#3420=VECTOR('',#12077,1.);
#3421=VECTOR('',#12080,1.);
#3422=VECTOR('',#12085,1.);
#3423=VECTOR('',#12086,1.);
#3424=VECTOR('',#12099,0.305);
#3425=VECTOR('',#12106,0.5);
#3426=VECTOR('',#12119,0.305);
#3427=VECTOR('',#12126,0.5);
#3428=VECTOR('',#12147,0.305);
#3429=VECTOR('',#12154,1.);
#3430=VECTOR('',#12155,1.);
#3431=VECTOR('',#12156,1.);
#3432=VECTOR('',#12157,1.);
#3433=VECTOR('',#12160,1.);
#3434=VECTOR('',#12161,1.);
#3435=VECTOR('',#12162,1.);
#3436=VECTOR('',#12163,1.);
#3437=VECTOR('',#12164,1.);
#3438=VECTOR('',#12167,1.);
#3439=VECTOR('',#12172,1.);
#3440=VECTOR('',#12173,1.);
#3441=VECTOR('',#12174,1.);
#3442=VECTOR('',#12175,1.);
#3443=VECTOR('',#12178,1.);
#3444=VECTOR('',#12179,1.);
#3445=VECTOR('',#12180,1.);
#3446=VECTOR('',#12183,1.);
#3447=VECTOR('',#12184,1.);
#3448=VECTOR('',#12185,1.);
#3449=VECTOR('',#12194,0.6);
#3450=VECTOR('',#12205,1.2);
#3451=VECTOR('',#12214,1.);
#3452=VECTOR('',#12221,0.165);
#3453=VECTOR('',#12228,1.);
#3454=VECTOR('',#12233,0.305);
#3455=VECTOR('',#12238,1.);
#3456=VECTOR('',#12239,1.);
#3457=VECTOR('',#12240,1.);
#3458=VECTOR('',#12241,1.);
#3459=VECTOR('',#12244,1.);
#3460=VECTOR('',#12245,1.);
#3461=VECTOR('',#12246,1.);
#3462=VECTOR('',#12249,1.);
#3463=VECTOR('',#12250,1.);
#3464=VECTOR('',#12253,1.);
#3465=VECTOR('',#12254,1.);
#3466=VECTOR('',#12257,1.);
#3467=VECTOR('',#12270,0.5);
#3468=VECTOR('',#12279,0.3);
#3469=VECTOR('',#12288,1.);
#3470=VECTOR('',#12299,1.);
#3471=VECTOR('',#12300,1.);
#3472=VECTOR('',#12301,1.);
#3473=VECTOR('',#12302,1.);
#3474=VECTOR('',#12305,1.);
#3475=VECTOR('',#12306,1.);
#3476=VECTOR('',#12307,1.);
#3477=VECTOR('',#12310,1.);
#3478=VECTOR('',#12311,1.);
#3479=VECTOR('',#12312,1.);
#3480=VECTOR('',#12315,1.);
#3481=VECTOR('',#12316,1.);
#3482=VECTOR('',#12317,1.);
#3483=VECTOR('',#12320,1.);
#3484=VECTOR('',#12321,1.);
#3485=VECTOR('',#12322,1.);
#3486=VECTOR('',#12325,1.);
#3487=VECTOR('',#12326,1.);
#3488=VECTOR('',#12337,0.185);
#3489=VECTOR('',#12342,0.2);
#3490=VECTOR('',#12347,0.1625);
#3491=CIRCLE('',#8767,0.225);
#3492=CIRCLE('',#8768,0.225);
#3493=CIRCLE('',#8770,0.225);
#3494=CIRCLE('',#8771,0.225);
#3495=CIRCLE('',#8773,0.225);
#3496=CIRCLE('',#8774,0.225);
#3497=CIRCLE('',#8776,0.225);
#3498=CIRCLE('',#8777,0.225);
#3499=CIRCLE('',#8779,0.21);
#3500=CIRCLE('',#8780,0.21);
#3501=CIRCLE('',#8782,0.210000000000001);
#3502=CIRCLE('',#8783,0.210000000000001);
#3503=CIRCLE('',#8785,0.210000000000001);
#3504=CIRCLE('',#8786,0.210000000000001);
#3505=CIRCLE('',#8788,0.21);
#3506=CIRCLE('',#8789,0.21);
#3507=CIRCLE('',#8791,0.275);
#3508=CIRCLE('',#8792,0.275);
#3509=CIRCLE('',#8794,0.275);
#3510=CIRCLE('',#8795,0.275);
#3511=CIRCLE('',#8797,0.275);
#3512=CIRCLE('',#8798,0.275);
#3513=CIRCLE('',#8800,0.275);
#3514=CIRCLE('',#8801,0.275);
#3515=CIRCLE('',#8810,0.275);
#3516=CIRCLE('',#8811,0.275);
#3517=CIRCLE('',#8813,0.275);
#3518=CIRCLE('',#8814,0.275);
#3519=CIRCLE('',#8816,0.275);
#3520=CIRCLE('',#8817,0.275);
#3521=CIRCLE('',#8819,0.275);
#3522=CIRCLE('',#8820,0.275);
#3523=CIRCLE('',#8843,0.225);
#3524=CIRCLE('',#8844,0.225);
#3525=CIRCLE('',#8846,0.165);
#3526=CIRCLE('',#8847,0.165);
#3527=CIRCLE('',#8850,0.165);
#3528=CIRCLE('',#8851,0.165);
#3529=CIRCLE('',#8854,0.165);
#3530=CIRCLE('',#8855,0.165);
#3531=CIRCLE('',#8858,0.165);
#3532=CIRCLE('',#8859,0.165);
#3533=CIRCLE('',#8862,0.165);
#3534=CIRCLE('',#8863,0.165);
#3535=CIRCLE('',#8865,0.165);
#3536=CIRCLE('',#8866,0.165);
#3537=CIRCLE('',#8868,0.165);
#3538=CIRCLE('',#8869,0.165);
#3539=CIRCLE('',#8871,0.165);
#3540=CIRCLE('',#8872,0.165);
#3541=CIRCLE('',#8874,0.275);
#3542=CIRCLE('',#8875,0.275);
#3543=CIRCLE('',#8877,0.275);
#3544=CIRCLE('',#8878,0.275);
#3545=CIRCLE('',#8880,0.275);
#3546=CIRCLE('',#8881,0.275);
#3547=CIRCLE('',#8883,0.275);
#3548=CIRCLE('',#8884,0.275);
#3549=CIRCLE('',#8886,1.05);
#3550=CIRCLE('',#8887,1.05);
#3551=CIRCLE('',#8889,0.625);
#3552=CIRCLE('',#8891,0.625);
#3553=CIRCLE('',#8893,1.5);
#3554=CIRCLE('',#8894,1.5);
#3555=CIRCLE('',#8896,2.);
#3556=CIRCLE('',#8897,2.);
#3557=CIRCLE('',#8899,2.2);
#3558=CIRCLE('',#8908,2.2);
#3559=CIRCLE('',#8918,0.225);
#3560=CIRCLE('',#8919,0.225);
#3561=CIRCLE('',#8921,0.225);
#3562=CIRCLE('',#8922,0.225);
#3563=CIRCLE('',#8924,0.225);
#3564=CIRCLE('',#8925,0.225);
#3565=CIRCLE('',#8927,0.225);
#3566=CIRCLE('',#8928,0.225);
#3567=CIRCLE('',#8930,1.49);
#3568=CIRCLE('',#8931,1.49);
#3569=CIRCLE('',#8933,0.71);
#3570=CIRCLE('',#8935,0.71);
#3571=CIRCLE('',#8937,2.2);
#3572=CIRCLE('',#8938,2.2);
#3573=CIRCLE('',#8943,0.225);
#3574=CIRCLE('',#8944,0.225);
#3575=CIRCLE('',#8946,0.225);
#3576=CIRCLE('',#8947,0.225);
#3577=CIRCLE('',#8949,0.225);
#3578=CIRCLE('',#8950,0.225);
#3579=CIRCLE('',#8952,0.225);
#3580=CIRCLE('',#8953,0.225);
#3581=CIRCLE('',#8955,1.49);
#3582=CIRCLE('',#8956,1.49);
#3583=CIRCLE('',#8958,0.71);
#3584=CIRCLE('',#8960,0.71);
#3585=CIRCLE('',#8962,2.2);
#3586=CIRCLE('',#8963,2.2);
#3587=CIRCLE('',#8968,0.375);
#3588=CIRCLE('',#8969,0.375);
#3589=CIRCLE('',#8971,0.225);
#3590=CIRCLE('',#8973,0.375);
#3591=CIRCLE('',#8974,0.375);
#3592=CIRCLE('',#8976,0.225);
#3593=CIRCLE('',#8978,0.375);
#3594=CIRCLE('',#8979,0.375);
#3595=CIRCLE('',#8981,0.225);
#3596=CIRCLE('',#8983,0.375);
#3597=CIRCLE('',#8984,0.375);
#3598=CIRCLE('',#8986,0.225);
#3599=CIRCLE('',#8988,0.225);
#3600=CIRCLE('',#8990,0.225);
#3601=CIRCLE('',#8992,0.225);
#3602=CIRCLE('',#8994,0.225);
#3603=CIRCLE('',#8996,1.04);
#3604=CIRCLE('',#8997,1.04);
#3605=CIRCLE('',#8999,0.625);
#3606=CIRCLE('',#9001,0.625);
#3607=CIRCLE('',#9003,2.);
#3608=CIRCLE('',#9004,2.);
#3609=CIRCLE('',#9016,0.165);
#3610=CIRCLE('',#9017,0.165);
#3611=CIRCLE('',#9020,0.165);
#3612=CIRCLE('',#9021,0.165);
#3613=CIRCLE('',#9031,0.165);
#3614=CIRCLE('',#9032,0.165);
#3615=CIRCLE('',#9035,0.165);
#3616=CIRCLE('',#9036,0.165);
#3617=CIRCLE('',#9046,0.165);
#3618=CIRCLE('',#9047,0.165);
#3619=CIRCLE('',#9050,0.5);
#3620=CIRCLE('',#9051,0.3);
#3621=CIRCLE('',#9053,0.5);
#3622=CIRCLE('',#9056,0.3);
#3623=CIRCLE('',#9096,0.21);
#3624=CIRCLE('',#9097,0.21);
#3625=CIRCLE('',#9112,0.2117);
#3626=CIRCLE('',#9121,0.2117);
#3627=CIRCLE('',#9122,0.2117);
#3628=CIRCLE('',#9124,0.2117);
#3629=CIRCLE('',#9131,0.285);
#3630=CIRCLE('',#9132,0.265);
#3631=CIRCLE('',#9134,0.265);
#3632=CIRCLE('',#9136,0.5);
#3633=CIRCLE('',#9138,0.5);
#3634=CIRCLE('',#9150,0.24505);
#3635=CIRCLE('',#9152,0.375);
#3636=CIRCLE('',#9154,0.425);
#3637=CIRCLE('',#9156,0.425);
#3638=CIRCLE('',#9158,0.395);
#3639=CIRCLE('',#9160,0.27);
#3640=CIRCLE('',#9162,0.24505);
#3641=CIRCLE('',#9167,0.976185);
#3642=CIRCLE('',#9168,0.976185);
#3643=CIRCLE('',#9169,0.247676);
#3644=CIRCLE('',#9170,0.976185);
#3645=CIRCLE('',#9171,0.976185);
#3646=CIRCLE('',#9173,0.976185);
#3647=CIRCLE('',#9175,0.5);
#3648=CIRCLE('',#9176,0.5);
#3649=CIRCLE('',#9178,0.56);
#3650=CIRCLE('',#9181,0.976185);
#3651=CIRCLE('',#9183,0.56);
#3652=CIRCLE('',#9187,1.023815);
#3653=CIRCLE('',#9188,1.023815);
#3654=CIRCLE('',#9189,0.247676);
#3655=CIRCLE('',#9190,1.023815);
#3656=CIRCLE('',#9191,1.023815);
#3657=CIRCLE('',#9193,1.023815);
#3658=CIRCLE('',#9195,1.44);
#3659=CIRCLE('',#9196,1.023815);
#3660=CIRCLE('',#9198,1.5);
#3661=CIRCLE('',#9200,1.5);
#3662=CIRCLE('',#9202,1.44);
#3663=CIRCLE('',#9207,0.23815);
#3664=CIRCLE('',#9209,0.23815);
#3665=CIRCLE('',#9211,0.23815);
#3666=CIRCLE('',#9213,0.23815);
#3667=CIRCLE('',#9215,0.23815);
#3668=CIRCLE('',#9217,0.23815);
#3669=CIRCLE('',#9219,0.23815);
#3670=CIRCLE('',#9221,0.23815);
#3671=CIRCLE('',#9224,0.243053047864041);
#3672=CIRCLE('',#9225,0.243053047864041);
#3673=CIRCLE('',#9227,1.019052);
#3674=CIRCLE('',#9228,1.019052);
#3675=CIRCLE('',#9229,1.019052);
#3676=CIRCLE('',#9230,1.019052);
#3677=CIRCLE('',#9231,1.019052);
#3678=CIRCLE('',#9232,1.019052);
#3679=CIRCLE('',#9233,1.019052);
#3680=CIRCLE('',#9234,1.019052);
#3681=CIRCLE('',#9235,1.019052);
#3682=CIRCLE('',#9237,0.980948);
#3683=CIRCLE('',#9238,0.243053047864041);
#3684=CIRCLE('',#9240,0.243053047864041);
#3685=CIRCLE('',#9242,0.980948);
#3686=CIRCLE('',#9243,0.243053047864041);
#3687=CIRCLE('',#9245,0.243053047864041);
#3688=CIRCLE('',#9247,0.980948);
#3689=CIRCLE('',#9248,0.243053047864041);
#3690=CIRCLE('',#9250,0.243053047864041);
#3691=CIRCLE('',#9252,0.980948);
#3692=CIRCLE('',#9253,0.243053047864041);
#3693=CIRCLE('',#9255,0.243053047864041);
#3694=CIRCLE('',#9257,0.980948);
#3695=CIRCLE('',#9258,0.243053047864041);
#3696=CIRCLE('',#9260,0.243053047864041);
#3697=CIRCLE('',#9262,0.980948);
#3698=CIRCLE('',#9263,0.243053047864041);
#3699=CIRCLE('',#9265,0.243053047864041);
#3700=CIRCLE('',#9267,0.980948);
#3701=CIRCLE('',#9268,0.980948);
#3702=CIRCLE('',#9269,0.980948);
#3703=CIRCLE('',#9271,0.243053047864041);
#3704=CIRCLE('',#9273,0.243053047864041);
#3705=CIRCLE('',#9278,1.013815);
#3706=CIRCLE('',#9279,0.991185);
#3707=CIRCLE('',#9281,1.013815);
#3708=CIRCLE('',#9283,0.991185);
#3709=CIRCLE('',#9286,1.013815);
#3710=CIRCLE('',#9287,0.991185);
#3711=CIRCLE('',#9289,1.013815);
#3712=CIRCLE('',#9291,0.991185);
#3713=CIRCLE('',#9301,0.9);
#3714=CIRCLE('',#9304,0.9);
#3715=CIRCLE('',#9308,1.05);
#3716=CIRCLE('',#9309,0.9);
#3717=CIRCLE('',#9311,1.05);
#3718=CIRCLE('',#9313,1.);
#3719=CIRCLE('',#9315,1.);
#3720=CIRCLE('',#9317,1.05);
#3721=CIRCLE('',#9319,1.05);
#3722=CIRCLE('',#9321,1.);
#3723=CIRCLE('',#9323,1.);
#3724=CIRCLE('',#9325,1.05);
#3725=CIRCLE('',#9327,1.05);
#3726=CIRCLE('',#9329,0.9);
#3727=CIRCLE('',#9333,0.895);
#3728=CIRCLE('',#9334,0.605);
#3729=CIRCLE('',#9337,0.895);
#3730=CIRCLE('',#9338,0.605);
#3731=CIRCLE('',#9341,0.895);
#3732=CIRCLE('',#9342,0.605);
#3733=CIRCLE('',#9344,0.895);
#3734=CIRCLE('',#9346,0.605);
#3735=CIRCLE('',#9360,0.2);
#3736=CIRCLE('',#9361,0.16);
#3737=CIRCLE('',#9363,0.2);
#3738=CIRCLE('',#9366,0.3);
#3739=CIRCLE('',#9368,0.35);
#3740=CIRCLE('',#9370,0.35);
#3741=CIRCLE('',#9372,0.32);
#3742=CIRCLE('',#9374,0.22);
#3743=CIRCLE('',#9376,0.1954);
#3744=CIRCLE('',#9378,0.1954);
#3745=CIRCLE('',#9383,0.305);
#3746=CIRCLE('',#9384,0.305);
#3747=CIRCLE('',#9386,0.8);
#3748=CIRCLE('',#9387,0.8);
#3749=CIRCLE('',#9389,1.);
#3750=CIRCLE('',#9390,1.);
#3751=CIRCLE('',#9391,0.7);
#3752=CIRCLE('',#9392,1.);
#3753=CIRCLE('',#9393,0.5);
#3754=CIRCLE('',#9396,1.);
#3755=CIRCLE('',#9399,0.7);
#3756=CIRCLE('',#9402,1.);
#3757=CIRCLE('',#9405,1.);
#3758=CIRCLE('',#9406,0.7);
#3759=CIRCLE('',#9409,0.7);
#3760=CIRCLE('',#9410,0.5);
#3761=CIRCLE('',#9413,0.5);
#3762=CIRCLE('',#9415,0.5);
#3763=CIRCLE('',#9420,0.505);
#3764=CIRCLE('',#9421,0.505);
#3765=CIRCLE('',#9423,0.7);
#3766=CIRCLE('',#9424,0.7);
#3767=CIRCLE('',#9429,0.164999999999999);
#3768=CIRCLE('',#9431,0.164999999999999);
#3769=CIRCLE('',#9432,0.164999999999999);
#3770=CIRCLE('',#9435,0.505);
#3771=CIRCLE('',#9436,0.505);
#3772=CIRCLE('',#9438,0.9);
#3773=CIRCLE('',#9439,0.9);
#3774=CIRCLE('',#9444,0.165);
#3775=CIRCLE('',#9445,0.165);
#3776=CIRCLE('',#9448,0.165);
#3777=CIRCLE('',#9449,0.165);
#3778=CIRCLE('',#9452,0.7);
#3779=CIRCLE('',#9453,0.3);
#3780=CIRCLE('',#9455,0.7);
#3781=CIRCLE('',#9456,0.3);
#3782=CIRCLE('',#9459,0.3);
#3783=CIRCLE('',#9461,0.3);
#3784=CIRCLE('',#9466,0.305);
#3785=CIRCLE('',#9467,0.305);
#3786=CIRCLE('',#9469,0.5);
#3787=CIRCLE('',#9470,0.5);
#3788=CIRCLE('',#9475,0.305);
#3789=CIRCLE('',#9476,0.305);
#3790=CIRCLE('',#9478,0.5);
#3791=CIRCLE('',#9479,0.5);
#3792=CIRCLE('',#9484,0.225);
#3793=CIRCLE('',#9485,0.225);
#3794=CIRCLE('',#9487,0.5);
#3795=CIRCLE('',#9488,0.5);
#3796=CIRCLE('',#9493,0.225);
#3797=CIRCLE('',#9494,0.225);
#3798=CIRCLE('',#9496,0.5);
#3799=CIRCLE('',#9497,0.5);
#3800=CIRCLE('',#9502,0.1954);
#3801=CIRCLE('',#9511,0.17);
#3802=CIRCLE('',#9513,0.1954);
#3803=CIRCLE('',#9525,0.1954);
#3804=CIRCLE('',#9527,0.3);
#3805=CIRCLE('',#9529,0.35);
#3806=CIRCLE('',#9531,0.35);
#3807=CIRCLE('',#9533,0.32);
#3808=CIRCLE('',#9535,0.22);
#3809=CIRCLE('',#9537,0.1954);
#3810=CIRCLE('',#9541,0.3);
#3811=CIRCLE('',#9543,0.35);
#3812=CIRCLE('',#9545,0.35);
#3813=CIRCLE('',#9547,0.32);
#3814=CIRCLE('',#9549,0.22);
#3815=CIRCLE('',#9551,0.1954);
#3816=CIRCLE('',#9553,0.1954);
#3817=CIRCLE('',#9555,0.16);
#3818=CIRCLE('',#9636,0.5);
#3819=CIRCLE('',#9637,0.5);
#3820=CIRCLE('',#9639,0.5);
#3821=CIRCLE('',#9640,0.5);
#3822=CIRCLE('',#9642,0.8);
#3823=CIRCLE('',#9643,0.8);
#3824=CIRCLE('',#9646,0.8);
#3825=CIRCLE('',#9649,0.8);
#3826=CIRCLE('',#9653,0.305);
#3827=CIRCLE('',#9654,0.305);
#3828=CIRCLE('',#9656,0.5);
#3829=CIRCLE('',#9657,0.5);
#3830=CIRCLE('',#9662,0.305);
#3831=CIRCLE('',#9663,0.305);
#3832=CIRCLE('',#9665,0.5);
#3833=CIRCLE('',#9666,0.5);
#3834=CIRCLE('',#9675,0.305);
#3835=CIRCLE('',#9676,0.305);
#3836=CIRCLE('',#9681,1.2);
#3837=CIRCLE('',#9686,0.6);
#3838=CIRCLE('',#9688,0.6);
#3839=CIRCLE('',#9689,0.6);
#3840=CIRCLE('',#9691,1.2);
#3841=CIRCLE('',#9692,1.2);
#3842=CIRCLE('',#9694,1.2);
#3843=CIRCLE('',#9698,0.165);
#3844=CIRCLE('',#9700,0.165);
#3845=CIRCLE('',#9701,0.165);
#3846=CIRCLE('',#9702,0.165);
#3847=CIRCLE('',#9705,0.305);
#3848=CIRCLE('',#9706,0.305);
#3849=CIRCLE('',#9715,0.5);
#3850=CIRCLE('',#9716,0.3);
#3851=CIRCLE('',#9718,0.5);
#3852=CIRCLE('',#9721,0.3);
#3853=CIRCLE('',#9725,1.);
#3854=CIRCLE('',#9726,1.);
#3855=CIRCLE('',#9738,0.17);
#3856=CIRCLE('',#9740,0.1954);
#3857=CIRCLE('',#9742,0.1954);
#3858=CIRCLE('',#9744,0.125);
#3859=VERTEX_POINT('',#12370);
#3860=VERTEX_POINT('',#12372);
#3861=VERTEX_POINT('',#12376);
#3862=VERTEX_POINT('',#12378);
#3863=VERTEX_POINT('',#12382);
#3864=VERTEX_POINT('',#12384);
#3865=VERTEX_POINT('',#12388);
#3866=VERTEX_POINT('',#12390);
#3867=VERTEX_POINT('',#12394);
#3868=VERTEX_POINT('',#12396);
#3869=VERTEX_POINT('',#12400);
#3870=VERTEX_POINT('',#12402);
#3871=VERTEX_POINT('',#12406);
#3872=VERTEX_POINT('',#12408);
#3873=VERTEX_POINT('',#12412);
#3874=VERTEX_POINT('',#12414);
#3875=VERTEX_POINT('',#12418);
#3876=VERTEX_POINT('',#12420);
#3877=VERTEX_POINT('',#12424);
#3878=VERTEX_POINT('',#12426);
#3879=VERTEX_POINT('',#12430);
#3880=VERTEX_POINT('',#12432);
#3881=VERTEX_POINT('',#12436);
#3882=VERTEX_POINT('',#12438);
#3883=VERTEX_POINT('',#12442);
#3884=VERTEX_POINT('',#12443);
#3885=VERTEX_POINT('',#12445);
#3886=VERTEX_POINT('',#12447);
#3887=VERTEX_POINT('',#12451);
#3888=VERTEX_POINT('',#12453);
#3889=VERTEX_POINT('',#12457);
#3890=VERTEX_POINT('',#12459);
#3891=VERTEX_POINT('',#12469);
#3892=VERTEX_POINT('',#12471);
#3893=VERTEX_POINT('',#12475);
#3894=VERTEX_POINT('',#12477);
#3895=VERTEX_POINT('',#12481);
#3896=VERTEX_POINT('',#12483);
#3897=VERTEX_POINT('',#12487);
#3898=VERTEX_POINT('',#12489);
#3899=VERTEX_POINT('',#12493);
#3900=VERTEX_POINT('',#12494);
#3901=VERTEX_POINT('',#12496);
#3902=VERTEX_POINT('',#12498);
#3903=VERTEX_POINT('',#12502);
#3904=VERTEX_POINT('',#12504);
#3905=VERTEX_POINT('',#12508);
#3906=VERTEX_POINT('',#12510);
#3907=VERTEX_POINT('',#12520);
#3908=VERTEX_POINT('',#12521);
#3909=VERTEX_POINT('',#12523);
#3910=VERTEX_POINT('',#12525);
#3911=VERTEX_POINT('',#12529);
#3912=VERTEX_POINT('',#12531);
#3913=VERTEX_POINT('',#12535);
#3914=VERTEX_POINT('',#12537);
#3915=VERTEX_POINT('',#12547);
#3916=VERTEX_POINT('',#12548);
#3917=VERTEX_POINT('',#12550);
#3918=VERTEX_POINT('',#12552);
#3919=VERTEX_POINT('',#12556);
#3920=VERTEX_POINT('',#12558);
#3921=VERTEX_POINT('',#12562);
#3922=VERTEX_POINT('',#12564);
#3923=VERTEX_POINT('',#12574);
#3924=VERTEX_POINT('',#12576);
#3925=VERTEX_POINT('',#12580);
#3926=VERTEX_POINT('',#12582);
#3927=VERTEX_POINT('',#12587);
#3928=VERTEX_POINT('',#12589);
#3929=VERTEX_POINT('',#12594);
#3930=VERTEX_POINT('',#12596);
#3931=VERTEX_POINT('',#12601);
#3932=VERTEX_POINT('',#12603);
#3933=VERTEX_POINT('',#12608);
#3934=VERTEX_POINT('',#12610);
#3935=VERTEX_POINT('',#12614);
#3936=VERTEX_POINT('',#12616);
#3937=VERTEX_POINT('',#12620);
#3938=VERTEX_POINT('',#12622);
#3939=VERTEX_POINT('',#12626);
#3940=VERTEX_POINT('',#12628);
#3941=VERTEX_POINT('',#12632);
#3942=VERTEX_POINT('',#12634);
#3943=VERTEX_POINT('',#12638);
#3944=VERTEX_POINT('',#12640);
#3945=VERTEX_POINT('',#12644);
#3946=VERTEX_POINT('',#12646);
#3947=VERTEX_POINT('',#12650);
#3948=VERTEX_POINT('',#12652);
#3949=VERTEX_POINT('',#12656);
#3950=VERTEX_POINT('',#12658);
#3951=VERTEX_POINT('',#12662);
#3952=VERTEX_POINT('',#12665);
#3953=VERTEX_POINT('',#12669);
#3954=VERTEX_POINT('',#12671);
#3955=VERTEX_POINT('',#12675);
#3956=VERTEX_POINT('',#12676);
#3957=VERTEX_POINT('',#12678);
#3958=VERTEX_POINT('',#12680);
#3959=VERTEX_POINT('',#12684);
#3960=VERTEX_POINT('',#12686);
#3961=VERTEX_POINT('',#12688);
#3962=VERTEX_POINT('',#12690);
#3963=VERTEX_POINT('',#12692);
#3964=VERTEX_POINT('',#12694);
#3965=VERTEX_POINT('',#12696);
#3966=VERTEX_POINT('',#12698);
#3967=VERTEX_POINT('',#12702);
#3968=VERTEX_POINT('',#12706);
#3969=VERTEX_POINT('',#12707);
#3970=VERTEX_POINT('',#12709);
#3971=VERTEX_POINT('',#12711);
#3972=VERTEX_POINT('',#12714);
#3973=VERTEX_POINT('',#12715);
#3974=VERTEX_POINT('',#12720);
#3975=VERTEX_POINT('',#12721);
#3976=VERTEX_POINT('',#12726);
#3977=VERTEX_POINT('',#12730);
#3978=VERTEX_POINT('',#12736);
#3979=VERTEX_POINT('',#12740);
#3980=VERTEX_POINT('',#12742);
#3981=VERTEX_POINT('',#12748);
#3982=VERTEX_POINT('',#12750);
#3983=VERTEX_POINT('',#12763);
#3984=VERTEX_POINT('',#12765);
#3985=VERTEX_POINT('',#12769);
#3986=VERTEX_POINT('',#12771);
#3987=VERTEX_POINT('',#12775);
#3988=VERTEX_POINT('',#12777);
#3989=VERTEX_POINT('',#12781);
#3990=VERTEX_POINT('',#12783);
#3991=VERTEX_POINT('',#12787);
#3992=VERTEX_POINT('',#12789);
#3993=VERTEX_POINT('',#12793);
#3994=VERTEX_POINT('',#12796);
#3995=VERTEX_POINT('',#12800);
#3996=VERTEX_POINT('',#12802);
#3997=VERTEX_POINT('',#12809);
#3998=VERTEX_POINT('',#12811);
#3999=VERTEX_POINT('',#12815);
#4000=VERTEX_POINT('',#12817);
#4001=VERTEX_POINT('',#12821);
#4002=VERTEX_POINT('',#12823);
#4003=VERTEX_POINT('',#12827);
#4004=VERTEX_POINT('',#12829);
#4005=VERTEX_POINT('',#12833);
#4006=VERTEX_POINT('',#12835);
#4007=VERTEX_POINT('',#12839);
#4008=VERTEX_POINT('',#12842);
#4009=VERTEX_POINT('',#12846);
#4010=VERTEX_POINT('',#12848);
#4011=VERTEX_POINT('',#12855);
#4012=VERTEX_POINT('',#12857);
#4013=VERTEX_POINT('',#12861);
#4014=VERTEX_POINT('',#12864);
#4015=VERTEX_POINT('',#12866);
#4016=VERTEX_POINT('',#12870);
#4017=VERTEX_POINT('',#12873);
#4018=VERTEX_POINT('',#12875);
#4019=VERTEX_POINT('',#12879);
#4020=VERTEX_POINT('',#12882);
#4021=VERTEX_POINT('',#12884);
#4022=VERTEX_POINT('',#12888);
#4023=VERTEX_POINT('',#12891);
#4024=VERTEX_POINT('',#12895);
#4025=VERTEX_POINT('',#12899);
#4026=VERTEX_POINT('',#12903);
#4027=VERTEX_POINT('',#12907);
#4028=VERTEX_POINT('',#12909);
#4029=VERTEX_POINT('',#12913);
#4030=VERTEX_POINT('',#12916);
#4031=VERTEX_POINT('',#12920);
#4032=VERTEX_POINT('',#12922);
#4033=VERTEX_POINT('',#12929);
#4034=VERTEX_POINT('',#12930);
#4035=VERTEX_POINT('',#12932);
#4036=VERTEX_POINT('',#12934);
#4037=VERTEX_POINT('',#12938);
#4038=VERTEX_POINT('',#12940);
#4039=VERTEX_POINT('',#12944);
#4040=VERTEX_POINT('',#12946);
#4041=VERTEX_POINT('',#12956);
#4042=VERTEX_POINT('',#12958);
#4043=VERTEX_POINT('',#12963);
#4044=VERTEX_POINT('',#12965);
#4045=VERTEX_POINT('',#12970);
#4046=VERTEX_POINT('',#12971);
#4047=VERTEX_POINT('',#12973);
#4048=VERTEX_POINT('',#12975);
#4049=VERTEX_POINT('',#12979);
#4050=VERTEX_POINT('',#12981);
#4051=VERTEX_POINT('',#12985);
#4052=VERTEX_POINT('',#12987);
#4053=VERTEX_POINT('',#12997);
#4054=VERTEX_POINT('',#12999);
#4055=VERTEX_POINT('',#13004);
#4056=VERTEX_POINT('',#13006);
#4057=VERTEX_POINT('',#13011);
#4058=VERTEX_POINT('',#13012);
#4059=VERTEX_POINT('',#13014);
#4060=VERTEX_POINT('',#13016);
#4061=VERTEX_POINT('',#13020);
#4062=VERTEX_POINT('',#13022);
#4063=VERTEX_POINT('',#13026);
#4064=VERTEX_POINT('',#13028);
#4065=VERTEX_POINT('',#13038);
#4066=VERTEX_POINT('',#13040);
#4067=VERTEX_POINT('',#13045);
#4068=VERTEX_POINT('',#13047);
#4069=VERTEX_POINT('',#13050);
#4070=VERTEX_POINT('',#13055);
#4071=VERTEX_POINT('',#13061);
#4072=VERTEX_POINT('',#13062);
#4073=VERTEX_POINT('',#13064);
#4074=VERTEX_POINT('',#13066);
#4075=VERTEX_POINT('',#13070);
#4076=VERTEX_POINT('',#13072);
#4077=VERTEX_POINT('',#13076);
#4078=VERTEX_POINT('',#13078);
#4079=VERTEX_POINT('',#13082);
#4080=VERTEX_POINT('',#13084);
#4081=VERTEX_POINT('',#13088);
#4082=VERTEX_POINT('',#13090);
#4083=VERTEX_POINT('',#13094);
#4084=VERTEX_POINT('',#13096);
#4085=VERTEX_POINT('',#13100);
#4086=VERTEX_POINT('',#13102);
#4087=VERTEX_POINT('',#13106);
#4088=VERTEX_POINT('',#13108);
#4089=VERTEX_POINT('',#13112);
#4090=VERTEX_POINT('',#13114);
#4091=VERTEX_POINT('',#13118);
#4092=VERTEX_POINT('',#13119);
#4093=VERTEX_POINT('',#13121);
#4094=VERTEX_POINT('',#13123);
#4095=VERTEX_POINT('',#13127);
#4096=VERTEX_POINT('',#13129);
#4097=VERTEX_POINT('',#13133);
#4098=VERTEX_POINT('',#13135);
#4099=VERTEX_POINT('',#13139);
#4100=VERTEX_POINT('',#13141);
#4101=VERTEX_POINT('',#13145);
#4102=VERTEX_POINT('',#13147);
#4103=VERTEX_POINT('',#13151);
#4104=VERTEX_POINT('',#13153);
#4105=VERTEX_POINT('',#13157);
#4106=VERTEX_POINT('',#13159);
#4107=VERTEX_POINT('',#13163);
#4108=VERTEX_POINT('',#13165);
#4109=VERTEX_POINT('',#13169);
#4110=VERTEX_POINT('',#13171);
#4111=VERTEX_POINT('',#13175);
#4112=VERTEX_POINT('',#13176);
#4113=VERTEX_POINT('',#13178);
#4114=VERTEX_POINT('',#13180);
#4115=VERTEX_POINT('',#13184);
#4116=VERTEX_POINT('',#13186);
#4117=VERTEX_POINT('',#13190);
#4118=VERTEX_POINT('',#13192);
#4119=VERTEX_POINT('',#13196);
#4120=VERTEX_POINT('',#13198);
#4121=VERTEX_POINT('',#13202);
#4122=VERTEX_POINT('',#13204);
#4123=VERTEX_POINT('',#13208);
#4124=VERTEX_POINT('',#13210);
#4125=VERTEX_POINT('',#13214);
#4126=VERTEX_POINT('',#13216);
#4127=VERTEX_POINT('',#13220);
#4128=VERTEX_POINT('',#13222);
#4129=VERTEX_POINT('',#13226);
#4130=VERTEX_POINT('',#13228);
#4131=VERTEX_POINT('',#13232);
#4132=VERTEX_POINT('',#13233);
#4133=VERTEX_POINT('',#13235);
#4134=VERTEX_POINT('',#13237);
#4135=VERTEX_POINT('',#13241);
#4136=VERTEX_POINT('',#13243);
#4137=VERTEX_POINT('',#13247);
#4138=VERTEX_POINT('',#13249);
#4139=VERTEX_POINT('',#13253);
#4140=VERTEX_POINT('',#13255);
#4141=VERTEX_POINT('',#13259);
#4142=VERTEX_POINT('',#13261);
#4143=VERTEX_POINT('',#13265);
#4144=VERTEX_POINT('',#13267);
#4145=VERTEX_POINT('',#13271);
#4146=VERTEX_POINT('',#13273);
#4147=VERTEX_POINT('',#13277);
#4148=VERTEX_POINT('',#13279);
#4149=VERTEX_POINT('',#13283);
#4150=VERTEX_POINT('',#13285);
#4151=VERTEX_POINT('',#13289);
#4152=VERTEX_POINT('',#13291);
#4153=VERTEX_POINT('',#13295);
#4154=VERTEX_POINT('',#13297);
#4155=VERTEX_POINT('',#13301);
#4156=VERTEX_POINT('',#13303);
#4157=VERTEX_POINT('',#13310);
#4158=VERTEX_POINT('',#13312);
#4159=VERTEX_POINT('',#13319);
#4160=VERTEX_POINT('',#13321);
#4161=VERTEX_POINT('',#13334);
#4162=VERTEX_POINT('',#13335);
#4163=VERTEX_POINT('',#13337);
#4164=VERTEX_POINT('',#13339);
#4165=VERTEX_POINT('',#13343);
#4166=VERTEX_POINT('',#13345);
#4167=VERTEX_POINT('',#13349);
#4168=VERTEX_POINT('',#13351);
#4169=VERTEX_POINT('',#13354);
#4170=VERTEX_POINT('',#13357);
#4171=VERTEX_POINT('',#13359);
#4172=VERTEX_POINT('',#13361);
#4173=VERTEX_POINT('',#13363);
#4174=VERTEX_POINT('',#13365);
#4175=VERTEX_POINT('',#13367);
#4176=VERTEX_POINT('',#13371);
#4177=VERTEX_POINT('',#13375);
#4178=VERTEX_POINT('',#13379);
#4179=VERTEX_POINT('',#13381);
#4180=VERTEX_POINT('',#13383);
#4181=VERTEX_POINT('',#13385);
#4182=VERTEX_POINT('',#13391);
#4183=VERTEX_POINT('',#13393);
#4184=VERTEX_POINT('',#13397);
#4185=VERTEX_POINT('',#13400);
#4186=VERTEX_POINT('',#13402);
#4187=VERTEX_POINT('',#13414);
#4188=VERTEX_POINT('',#13416);
#4189=VERTEX_POINT('',#13420);
#4190=VERTEX_POINT('',#13424);
#4191=VERTEX_POINT('',#13427);
#4192=VERTEX_POINT('',#13433);
#4193=VERTEX_POINT('',#13434);
#4194=VERTEX_POINT('',#13436);
#4195=VERTEX_POINT('',#13438);
#4196=VERTEX_POINT('',#13442);
#4197=VERTEX_POINT('',#13444);
#4198=VERTEX_POINT('',#13448);
#4199=VERTEX_POINT('',#13450);
#4200=VERTEX_POINT('',#13454);
#4201=VERTEX_POINT('',#13456);
#4202=VERTEX_POINT('',#13460);
#4203=VERTEX_POINT('',#13462);
#4204=VERTEX_POINT('',#13471);
#4205=VERTEX_POINT('',#13474);
#4206=VERTEX_POINT('',#13477);
#4207=VERTEX_POINT('',#13481);
#4208=VERTEX_POINT('',#13485);
#4209=VERTEX_POINT('',#13489);
#4210=VERTEX_POINT('',#13492);
#4211=VERTEX_POINT('',#13500);
#4212=VERTEX_POINT('',#13501);
#4213=VERTEX_POINT('',#13504);
#4214=VERTEX_POINT('',#13506);
#4215=VERTEX_POINT('',#13510);
#4216=VERTEX_POINT('',#13514);
#4217=VERTEX_POINT('',#13516);
#4218=VERTEX_POINT('',#13520);
#4219=VERTEX_POINT('',#13525);
#4220=VERTEX_POINT('',#13529);
#4221=VERTEX_POINT('',#13535);
#4222=VERTEX_POINT('',#13536);
#4223=VERTEX_POINT('',#13539);
#4224=VERTEX_POINT('',#13541);
#4225=VERTEX_POINT('',#13545);
#4226=VERTEX_POINT('',#13549);
#4227=VERTEX_POINT('',#13551);
#4228=VERTEX_POINT('',#13554);
#4229=VERTEX_POINT('',#13558);
#4230=VERTEX_POINT('',#13562);
#4231=VERTEX_POINT('',#13570);
#4232=VERTEX_POINT('',#13571);
#4233=VERTEX_POINT('',#13574);
#4234=VERTEX_POINT('',#13575);
#4235=VERTEX_POINT('',#13578);
#4236=VERTEX_POINT('',#13579);
#4237=VERTEX_POINT('',#13582);
#4238=VERTEX_POINT('',#13583);
#4239=VERTEX_POINT('',#13586);
#4240=VERTEX_POINT('',#13587);
#4241=VERTEX_POINT('',#13590);
#4242=VERTEX_POINT('',#13591);
#4243=VERTEX_POINT('',#13594);
#4244=VERTEX_POINT('',#13595);
#4245=VERTEX_POINT('',#13598);
#4246=VERTEX_POINT('',#13599);
#4247=VERTEX_POINT('',#13603);
#4248=VERTEX_POINT('',#13604);
#4249=VERTEX_POINT('',#13627);
#4250=VERTEX_POINT('',#13629);
#4251=VERTEX_POINT('',#13654);
#4252=VERTEX_POINT('',#13656);
#4253=VERTEX_POINT('',#13679);
#4254=VERTEX_POINT('',#13681);
#4255=VERTEX_POINT('',#13704);
#4256=VERTEX_POINT('',#13706);
#4257=VERTEX_POINT('',#13719);
#4258=VERTEX_POINT('',#13722);
#4259=VERTEX_POINT('',#13735);
#4260=VERTEX_POINT('',#13737);
#4261=VERTEX_POINT('',#13760);
#4262=VERTEX_POINT('',#13762);
#4263=VERTEX_POINT('',#13785);
#4264=VERTEX_POINT('',#13787);
#4265=VERTEX_POINT('',#13810);
#4266=VERTEX_POINT('',#13812);
#4267=VERTEX_POINT('',#13837);
#4268=VERTEX_POINT('',#13841);
#4269=VERTEX_POINT('',#13866);
#4270=VERTEX_POINT('',#13870);
#4271=VERTEX_POINT('',#13895);
#4272=VERTEX_POINT('',#13899);
#4273=VERTEX_POINT('',#13900);
#4274=VERTEX_POINT('',#13927);
#4275=VERTEX_POINT('',#13931);
#4276=VERTEX_POINT('',#13956);
#4277=VERTEX_POINT('',#13960);
#4278=VERTEX_POINT('',#13985);
#4279=VERTEX_POINT('',#13989);
#4280=VERTEX_POINT('',#14014);
#4281=VERTEX_POINT('',#14017);
#4282=VERTEX_POINT('',#14019);
#4283=VERTEX_POINT('',#14051);
#4284=VERTEX_POINT('',#14053);
#4285=VERTEX_POINT('',#14056);
#4286=VERTEX_POINT('',#14060);
#4287=VERTEX_POINT('',#14065);
#4288=VERTEX_POINT('',#14067);
#4289=VERTEX_POINT('',#14070);
#4290=VERTEX_POINT('',#14074);
#4291=VERTEX_POINT('',#14086);
#4292=VERTEX_POINT('',#14087);
#4293=VERTEX_POINT('',#14089);
#4294=VERTEX_POINT('',#14091);
#4295=VERTEX_POINT('',#14095);
#4296=VERTEX_POINT('',#14097);
#4297=VERTEX_POINT('',#14101);
#4298=VERTEX_POINT('',#14103);
#4299=VERTEX_POINT('',#14111);
#4300=VERTEX_POINT('',#14113);
#4301=VERTEX_POINT('',#14116);
#4302=VERTEX_POINT('',#14120);
#4303=VERTEX_POINT('',#14123);
#4304=VERTEX_POINT('',#14127);
#4305=VERTEX_POINT('',#14130);
#4306=VERTEX_POINT('',#14134);
#4307=VERTEX_POINT('',#14137);
#4308=VERTEX_POINT('',#14141);
#4309=VERTEX_POINT('',#14144);
#4310=VERTEX_POINT('',#14148);
#4311=VERTEX_POINT('',#14154);
#4312=VERTEX_POINT('',#14155);
#4313=VERTEX_POINT('',#14157);
#4314=VERTEX_POINT('',#14159);
#4315=VERTEX_POINT('',#14163);
#4316=VERTEX_POINT('',#14165);
#4317=VERTEX_POINT('',#14169);
#4318=VERTEX_POINT('',#14171);
#4319=VERTEX_POINT('',#14178);
#4320=VERTEX_POINT('',#14180);
#4321=VERTEX_POINT('',#14183);
#4322=VERTEX_POINT('',#14187);
#4323=VERTEX_POINT('',#14195);
#4324=VERTEX_POINT('',#14196);
#4325=VERTEX_POINT('',#14198);
#4326=VERTEX_POINT('',#14200);
#4327=VERTEX_POINT('',#14204);
#4328=VERTEX_POINT('',#14206);
#4329=VERTEX_POINT('',#14210);
#4330=VERTEX_POINT('',#14212);
#4331=VERTEX_POINT('',#14216);
#4332=VERTEX_POINT('',#14218);
#4333=VERTEX_POINT('',#14222);
#4334=VERTEX_POINT('',#14224);
#4335=VERTEX_POINT('',#14233);
#4336=VERTEX_POINT('',#14235);
#4337=VERTEX_POINT('',#14238);
#4338=VERTEX_POINT('',#14243);
#4339=VERTEX_POINT('',#14246);
#4340=VERTEX_POINT('',#14250);
#4341=VERTEX_POINT('',#14254);
#4342=VERTEX_POINT('',#14258);
#4343=VERTEX_POINT('',#14261);
#4344=VERTEX_POINT('',#14265);
#4345=VERTEX_POINT('',#14273);
#4346=VERTEX_POINT('',#14275);
#4347=VERTEX_POINT('',#14279);
#4348=VERTEX_POINT('',#14280);
#4349=VERTEX_POINT('',#14282);
#4350=VERTEX_POINT('',#14284);
#4351=VERTEX_POINT('',#14288);
#4352=VERTEX_POINT('',#14290);
#4353=VERTEX_POINT('',#14292);
#4354=VERTEX_POINT('',#14294);
#4355=VERTEX_POINT('',#14296);
#4356=VERTEX_POINT('',#14298);
#4357=VERTEX_POINT('',#14300);
#4358=VERTEX_POINT('',#14303);
#4359=VERTEX_POINT('',#14306);
#4360=VERTEX_POINT('',#14310);
#4361=VERTEX_POINT('',#14316);
#4362=VERTEX_POINT('',#14318);
#4363=VERTEX_POINT('',#14322);
#4364=VERTEX_POINT('',#14326);
#4365=VERTEX_POINT('',#14332);
#4366=VERTEX_POINT('',#14334);
#4367=VERTEX_POINT('',#14339);
#4368=VERTEX_POINT('',#14341);
#4369=VERTEX_POINT('',#14346);
#4370=VERTEX_POINT('',#14350);
#4371=VERTEX_POINT('',#14357);
#4372=VERTEX_POINT('',#14359);
#4373=VERTEX_POINT('',#14363);
#4374=VERTEX_POINT('',#14365);
#4375=VERTEX_POINT('',#14372);
#4376=VERTEX_POINT('',#14373);
#4377=VERTEX_POINT('',#14377);
#4378=VERTEX_POINT('',#14392);
#4379=VERTEX_POINT('',#14394);
#4380=VERTEX_POINT('',#14396);
#4381=VERTEX_POINT('',#14433);
#4382=VERTEX_POINT('',#14452);
#4383=VERTEX_POINT('',#14454);
#4384=VERTEX_POINT('',#14458);
#4385=VERTEX_POINT('',#14460);
#4386=VERTEX_POINT('',#14467);
#4387=VERTEX_POINT('',#14469);
#4388=VERTEX_POINT('',#14474);
#4389=VERTEX_POINT('',#14476);
#4390=VERTEX_POINT('',#14481);
#4391=VERTEX_POINT('',#14483);
#4392=VERTEX_POINT('',#14486);
#4393=VERTEX_POINT('',#14488);
#4394=VERTEX_POINT('',#14493);
#4395=VERTEX_POINT('',#14497);
#4396=VERTEX_POINT('',#14504);
#4397=VERTEX_POINT('',#14506);
#4398=VERTEX_POINT('',#14510);
#4399=VERTEX_POINT('',#14512);
#4400=VERTEX_POINT('',#14519);
#4401=VERTEX_POINT('',#14521);
#4402=VERTEX_POINT('',#14525);
#4403=VERTEX_POINT('',#14527);
#4404=VERTEX_POINT('',#14534);
#4405=VERTEX_POINT('',#14536);
#4406=VERTEX_POINT('',#14540);
#4407=VERTEX_POINT('',#14542);
#4408=VERTEX_POINT('',#14549);
#4409=VERTEX_POINT('',#14551);
#4410=VERTEX_POINT('',#14555);
#4411=VERTEX_POINT('',#14557);
#4412=VERTEX_POINT('',#14564);
#4413=VERTEX_POINT('',#14567);
#4414=VERTEX_POINT('',#14568);
#4415=VERTEX_POINT('',#14570);
#4416=VERTEX_POINT('',#14572);
#4417=VERTEX_POINT('',#14576);
#4418=VERTEX_POINT('',#14578);
#4419=VERTEX_POINT('',#14582);
#4420=VERTEX_POINT('',#14584);
#4421=VERTEX_POINT('',#14588);
#4422=VERTEX_POINT('',#14590);
#4423=VERTEX_POINT('',#14594);
#4424=VERTEX_POINT('',#14596);
#4425=VERTEX_POINT('',#14604);
#4426=VERTEX_POINT('',#14607);
#4427=VERTEX_POINT('',#14614);
#4428=VERTEX_POINT('',#14615);
#4429=VERTEX_POINT('',#14617);
#4430=VERTEX_POINT('',#14619);
#4431=VERTEX_POINT('',#14623);
#4432=VERTEX_POINT('',#14625);
#4433=VERTEX_POINT('',#14629);
#4434=VERTEX_POINT('',#14631);
#4435=VERTEX_POINT('',#14635);
#4436=VERTEX_POINT('',#14637);
#4437=VERTEX_POINT('',#14641);
#4438=VERTEX_POINT('',#14643);
#4439=VERTEX_POINT('',#14652);
#4440=VERTEX_POINT('',#14655);
#4441=VERTEX_POINT('',#14658);
#4442=VERTEX_POINT('',#14662);
#4443=VERTEX_POINT('',#14666);
#4444=VERTEX_POINT('',#14670);
#4445=VERTEX_POINT('',#14673);
#4446=VERTEX_POINT('',#14680);
#4447=VERTEX_POINT('',#14683);
#4448=VERTEX_POINT('',#14687);
#4449=VERTEX_POINT('',#14691);
#4450=VERTEX_POINT('',#14695);
#4451=VERTEX_POINT('',#14698);
#4452=VERTEX_POINT('',#14702);
#4453=VERTEX_POINT('',#14706);
#4454=VERTEX_POINT('',#14711);
#4455=VERTEX_POINT('',#14712);
#4456=VERTEX_POINT('',#14714);
#4457=VERTEX_POINT('',#14716);
#4458=VERTEX_POINT('',#14720);
#4459=VERTEX_POINT('',#14722);
#4460=VERTEX_POINT('',#14726);
#4461=VERTEX_POINT('',#14728);
#4462=VERTEX_POINT('',#14732);
#4463=VERTEX_POINT('',#14734);
#4464=VERTEX_POINT('',#14738);
#4465=VERTEX_POINT('',#14740);
#4466=VERTEX_POINT('',#14819);
#4467=VERTEX_POINT('',#14821);
#4468=VERTEX_POINT('',#14825);
#4469=VERTEX_POINT('',#14827);
#4470=VERTEX_POINT('',#14831);
#4471=VERTEX_POINT('',#14832);
#4472=VERTEX_POINT('',#14834);
#4473=VERTEX_POINT('',#14836);
#4474=VERTEX_POINT('',#14840);
#4475=VERTEX_POINT('',#14842);
#4476=VERTEX_POINT('',#14846);
#4477=VERTEX_POINT('',#14850);
#4478=VERTEX_POINT('',#14858);
#4479=VERTEX_POINT('',#14860);
#4480=VERTEX_POINT('',#14864);
#4481=VERTEX_POINT('',#14866);
#4482=VERTEX_POINT('',#14873);
#4483=VERTEX_POINT('',#14875);
#4484=VERTEX_POINT('',#14879);
#4485=VERTEX_POINT('',#14881);
#4486=VERTEX_POINT('',#14892);
#4487=VERTEX_POINT('',#14894);
#4488=VERTEX_POINT('',#14899);
#4489=VERTEX_POINT('',#14900);
#4490=VERTEX_POINT('',#14902);
#4491=VERTEX_POINT('',#14904);
#4492=VERTEX_POINT('',#14908);
#4493=VERTEX_POINT('',#14910);
#4494=VERTEX_POINT('',#14912);
#4495=VERTEX_POINT('',#14914);
#4496=VERTEX_POINT('',#14918);
#4497=VERTEX_POINT('',#14922);
#4498=VERTEX_POINT('',#14924);
#4499=VERTEX_POINT('',#14926);
#4500=VERTEX_POINT('',#14930);
#4501=VERTEX_POINT('',#14931);
#4502=VERTEX_POINT('',#14936);
#4503=VERTEX_POINT('',#14938);
#4504=VERTEX_POINT('',#14944);
#4505=VERTEX_POINT('',#14949);
#4506=VERTEX_POINT('',#14953);
#4507=VERTEX_POINT('',#14959);
#4508=VERTEX_POINT('',#14960);
#4509=VERTEX_POINT('',#14964);
#4510=VERTEX_POINT('',#14975);
#4511=VERTEX_POINT('',#14977);
#4512=VERTEX_POINT('',#14980);
#4513=VERTEX_POINT('',#14995);
#4514=VERTEX_POINT('',#14997);
#4515=VERTEX_POINT('',#15001);
#4516=VERTEX_POINT('',#15002);
#4517=VERTEX_POINT('',#15004);
#4518=VERTEX_POINT('',#15006);
#4519=VERTEX_POINT('',#15010);
#4520=VERTEX_POINT('',#15011);
#4521=VERTEX_POINT('',#15016);
#4522=VERTEX_POINT('',#15020);
#4523=VERTEX_POINT('',#15028);
#4524=VERTEX_POINT('',#15030);
#4525=VERTEX_POINT('',#15033);
#4526=VERTEX_POINT('',#15038);
#4527=VERTEX_POINT('',#15044);
#4528=VERTEX_POINT('',#15046);
#4529=VERTEX_POINT('',#15053);
#4530=VERTEX_POINT('',#15054);
#4531=VERTEX_POINT('',#15056);
#4532=VERTEX_POINT('',#15058);
#4533=VERTEX_POINT('',#15062);
#4534=VERTEX_POINT('',#15064);
#4535=VERTEX_POINT('',#15068);
#4536=VERTEX_POINT('',#15070);
#4537=VERTEX_POINT('',#15074);
#4538=VERTEX_POINT('',#15076);
#4539=VERTEX_POINT('',#15080);
#4540=VERTEX_POINT('',#15082);
#4541=VERTEX_POINT('',#15090);
#4542=VERTEX_POINT('',#15093);
#4543=VERTEX_POINT('',#15097);
#4544=VERTEX_POINT('',#15101);
#4545=EDGE_CURVE('',#3859,#3859,#3491,.T.);
#4546=EDGE_CURVE('',#3859,#3860,#2231,.T.);
#4547=EDGE_CURVE('',#3860,#3860,#3492,.T.);
#4548=EDGE_CURVE('',#3861,#3861,#3493,.T.);
#4549=EDGE_CURVE('',#3861,#3862,#2232,.T.);
#4550=EDGE_CURVE('',#3862,#3862,#3494,.T.);
#4551=EDGE_CURVE('',#3863,#3863,#3495,.T.);
#4552=EDGE_CURVE('',#3863,#3864,#2233,.T.);
#4553=EDGE_CURVE('',#3864,#3864,#3496,.T.);
#4554=EDGE_CURVE('',#3865,#3865,#3497,.T.);
#4555=EDGE_CURVE('',#3865,#3866,#2234,.T.);
#4556=EDGE_CURVE('',#3866,#3866,#3498,.T.);
#4557=EDGE_CURVE('',#3867,#3867,#3499,.T.);
#4558=EDGE_CURVE('',#3867,#3868,#2235,.T.);
#4559=EDGE_CURVE('',#3868,#3868,#3500,.T.);
#4560=EDGE_CURVE('',#3869,#3869,#3501,.T.);
#4561=EDGE_CURVE('',#3869,#3870,#2236,.T.);
#4562=EDGE_CURVE('',#3870,#3870,#3502,.T.);
#4563=EDGE_CURVE('',#3871,#3871,#3503,.T.);
#4564=EDGE_CURVE('',#3871,#3872,#2237,.T.);
#4565=EDGE_CURVE('',#3872,#3872,#3504,.T.);
#4566=EDGE_CURVE('',#3873,#3873,#3505,.T.);
#4567=EDGE_CURVE('',#3873,#3874,#2238,.T.);
#4568=EDGE_CURVE('',#3874,#3874,#3506,.T.);
#4569=EDGE_CURVE('',#3875,#3875,#3507,.T.);
#4570=EDGE_CURVE('',#3875,#3876,#2239,.T.);
#4571=EDGE_CURVE('',#3876,#3876,#3508,.T.);
#4572=EDGE_CURVE('',#3877,#3877,#3509,.T.);
#4573=EDGE_CURVE('',#3877,#3878,#2240,.T.);
#4574=EDGE_CURVE('',#3878,#3878,#3510,.T.);
#4575=EDGE_CURVE('',#3879,#3879,#3511,.T.);
#4576=EDGE_CURVE('',#3879,#3880,#2241,.T.);
#4577=EDGE_CURVE('',#3880,#3880,#3512,.T.);
#4578=EDGE_CURVE('',#3881,#3881,#3513,.T.);
#4579=EDGE_CURVE('',#3881,#3882,#2242,.T.);
#4580=EDGE_CURVE('',#3882,#3882,#3514,.T.);
#4581=EDGE_CURVE('',#3883,#3884,#2243,.T.);
#4582=EDGE_CURVE('',#3884,#3885,#2244,.T.);
#4583=EDGE_CURVE('',#3886,#3885,#2245,.T.);
#4584=EDGE_CURVE('',#3883,#3886,#2246,.T.);
#4585=EDGE_CURVE('',#3887,#3883,#2247,.T.);
#4586=EDGE_CURVE('',#3888,#3886,#2248,.T.);
#4587=EDGE_CURVE('',#3887,#3888,#2249,.T.);
#4588=EDGE_CURVE('',#3889,#3887,#2250,.T.);
#4589=EDGE_CURVE('',#3890,#3888,#2251,.T.);
#4590=EDGE_CURVE('',#3889,#3890,#2252,.T.);
#4591=EDGE_CURVE('',#3884,#3889,#2253,.T.);
#4592=EDGE_CURVE('',#3885,#3890,#2254,.T.);
#4593=EDGE_CURVE('',#3891,#3891,#3515,.T.);
#4594=EDGE_CURVE('',#3891,#3892,#2255,.T.);
#4595=EDGE_CURVE('',#3892,#3892,#3516,.T.);
#4596=EDGE_CURVE('',#3893,#3893,#3517,.T.);
#4597=EDGE_CURVE('',#3893,#3894,#2256,.T.);
#4598=EDGE_CURVE('',#3894,#3894,#3518,.T.);
#4599=EDGE_CURVE('',#3895,#3895,#3519,.T.);
#4600=EDGE_CURVE('',#3895,#3896,#2257,.T.);
#4601=EDGE_CURVE('',#3896,#3896,#3520,.T.);
#4602=EDGE_CURVE('',#3897,#3897,#3521,.T.);
#4603=EDGE_CURVE('',#3897,#3898,#2258,.T.);
#4604=EDGE_CURVE('',#3898,#3898,#3522,.T.);
#4605=EDGE_CURVE('',#3899,#3900,#2259,.T.);
#4606=EDGE_CURVE('',#3900,#3901,#2260,.T.);
#4607=EDGE_CURVE('',#3902,#3901,#2261,.T.);
#4608=EDGE_CURVE('',#3899,#3902,#2262,.T.);
#4609=EDGE_CURVE('',#3903,#3899,#2263,.T.);
#4610=EDGE_CURVE('',#3904,#3902,#2264,.T.);
#4611=EDGE_CURVE('',#3903,#3904,#2265,.T.);
#4612=EDGE_CURVE('',#3905,#3903,#2266,.T.);
#4613=EDGE_CURVE('',#3906,#3904,#2267,.T.);
#4614=EDGE_CURVE('',#3905,#3906,#2268,.T.);
#4615=EDGE_CURVE('',#3900,#3905,#2269,.T.);
#4616=EDGE_CURVE('',#3901,#3906,#2270,.T.);
#4617=EDGE_CURVE('',#3907,#3908,#2271,.T.);
#4618=EDGE_CURVE('',#3908,#3909,#2272,.T.);
#4619=EDGE_CURVE('',#3910,#3909,#2273,.T.);
#4620=EDGE_CURVE('',#3907,#3910,#2274,.T.);
#4621=EDGE_CURVE('',#3911,#3907,#2275,.T.);
#4622=EDGE_CURVE('',#3912,#3910,#2276,.T.);
#4623=EDGE_CURVE('',#3911,#3912,#2277,.T.);
#4624=EDGE_CURVE('',#3913,#3911,#2278,.T.);
#4625=EDGE_CURVE('',#3914,#3912,#2279,.T.);
#4626=EDGE_CURVE('',#3913,#3914,#2280,.T.);
#4627=EDGE_CURVE('',#3908,#3913,#2281,.T.);
#4628=EDGE_CURVE('',#3909,#3914,#2282,.T.);
#4629=EDGE_CURVE('',#3915,#3916,#2283,.T.);
#4630=EDGE_CURVE('',#3916,#3917,#2284,.T.);
#4631=EDGE_CURVE('',#3918,#3917,#2285,.T.);
#4632=EDGE_CURVE('',#3915,#3918,#2286,.T.);
#4633=EDGE_CURVE('',#3919,#3915,#2287,.T.);
#4634=EDGE_CURVE('',#3920,#3918,#2288,.T.);
#4635=EDGE_CURVE('',#3919,#3920,#2289,.T.);
#4636=EDGE_CURVE('',#3921,#3919,#2290,.T.);
#4637=EDGE_CURVE('',#3922,#3920,#2291,.T.);
#4638=EDGE_CURVE('',#3921,#3922,#2292,.T.);
#4639=EDGE_CURVE('',#3916,#3921,#2293,.T.);
#4640=EDGE_CURVE('',#3917,#3922,#2294,.T.);
#4641=EDGE_CURVE('',#3923,#3923,#3523,.T.);
#4642=EDGE_CURVE('',#3923,#3924,#2295,.T.);
#4643=EDGE_CURVE('',#3924,#3924,#3524,.T.);
#4644=EDGE_CURVE('',#3925,#3925,#3525,.T.);
#4645=EDGE_CURVE('',#3925,#3926,#2296,.T.);
#4646=EDGE_CURVE('',#3926,#3926,#3526,.T.);
#4647=EDGE_CURVE('',#3927,#3927,#3527,.T.);
#4648=EDGE_CURVE('',#3927,#3928,#2297,.T.);
#4649=EDGE_CURVE('',#3928,#3928,#3528,.T.);
#4650=EDGE_CURVE('',#3929,#3929,#3529,.T.);
#4651=EDGE_CURVE('',#3929,#3930,#2298,.T.);
#4652=EDGE_CURVE('',#3930,#3930,#3530,.T.);
#4653=EDGE_CURVE('',#3931,#3931,#3531,.T.);
#4654=EDGE_CURVE('',#3931,#3932,#2299,.T.);
#4655=EDGE_CURVE('',#3932,#3932,#3532,.T.);
#4656=EDGE_CURVE('',#3933,#3933,#3533,.T.);
#4657=EDGE_CURVE('',#3933,#3934,#2300,.T.);
#4658=EDGE_CURVE('',#3934,#3934,#3534,.T.);
#4659=EDGE_CURVE('',#3935,#3935,#3535,.T.);
#4660=EDGE_CURVE('',#3935,#3936,#2301,.T.);
#4661=EDGE_CURVE('',#3936,#3936,#3536,.T.);
#4662=EDGE_CURVE('',#3937,#3937,#3537,.T.);
#4663=EDGE_CURVE('',#3937,#3938,#2302,.T.);
#4664=EDGE_CURVE('',#3938,#3938,#3538,.T.);
#4665=EDGE_CURVE('',#3939,#3939,#3539,.T.);
#4666=EDGE_CURVE('',#3939,#3940,#2303,.T.);
#4667=EDGE_CURVE('',#3940,#3940,#3540,.T.);
#4668=EDGE_CURVE('',#3941,#3941,#3541,.T.);
#4669=EDGE_CURVE('',#3941,#3942,#2304,.T.);
#4670=EDGE_CURVE('',#3942,#3942,#3542,.T.);
#4671=EDGE_CURVE('',#3943,#3943,#3543,.T.);
#4672=EDGE_CURVE('',#3943,#3944,#2305,.T.);
#4673=EDGE_CURVE('',#3944,#3944,#3544,.T.);
#4674=EDGE_CURVE('',#3945,#3945,#3545,.T.);
#4675=EDGE_CURVE('',#3945,#3946,#2306,.T.);
#4676=EDGE_CURVE('',#3946,#3946,#3546,.T.);
#4677=EDGE_CURVE('',#3947,#3947,#3547,.T.);
#4678=EDGE_CURVE('',#3947,#3948,#2307,.T.);
#4679=EDGE_CURVE('',#3948,#3948,#3548,.T.);
#4680=EDGE_CURVE('',#3949,#3949,#3549,.T.);
#4681=EDGE_CURVE('',#3949,#3950,#2308,.T.);
#4682=EDGE_CURVE('',#3950,#3950,#3550,.T.);
#4683=EDGE_CURVE('',#3951,#3951,#3551,.T.);
#4684=EDGE_CURVE('',#3952,#3952,#3552,.T.);
#4685=EDGE_CURVE('',#3952,#3951,#2309,.T.);
#4686=EDGE_CURVE('',#3953,#3953,#3553,.T.);
#4687=EDGE_CURVE('',#3953,#3954,#2310,.T.);
#4688=EDGE_CURVE('',#3954,#3954,#3554,.T.);
#4689=EDGE_CURVE('',#3955,#3956,#2311,.T.);
#4690=EDGE_CURVE('',#3955,#3957,#3555,.T.);
#4691=EDGE_CURVE('',#3958,#3957,#2312,.T.);
#4692=EDGE_CURVE('',#3956,#3958,#3556,.T.);
#4693=EDGE_CURVE('',#3956,#3959,#2313,.T.);
#4694=EDGE_CURVE('',#3959,#3960,#2314,.T.);
#4695=EDGE_CURVE('',#3961,#3960,#2315,.T.);
#4696=EDGE_CURVE('',#3962,#3961,#2316,.T.);
#4697=EDGE_CURVE('',#3962,#3963,#2317,.T.);
#4698=EDGE_CURVE('',#3963,#3964,#2318,.T.);
#4699=EDGE_CURVE('',#3964,#3965,#2319,.T.);
#4700=EDGE_CURVE('',#3966,#3965,#3557,.T.);
#4701=EDGE_CURVE('',#3966,#3955,#2320,.T.);
#4702=EDGE_CURVE('',#3967,#3958,#2321,.T.);
#4703=EDGE_CURVE('',#3959,#3967,#2322,.T.);
#4704=EDGE_CURVE('',#3968,#3969,#2323,.T.);
#4705=EDGE_CURVE('',#3969,#3970,#2324,.T.);
#4706=EDGE_CURVE('',#3970,#3971,#2325,.T.);
#4707=EDGE_CURVE('',#3971,#3968,#2326,.T.);
#4708=EDGE_CURVE('',#3972,#3973,#2327,.T.);
#4709=EDGE_CURVE('',#3963,#3972,#2328,.T.);
#4710=EDGE_CURVE('',#3973,#3962,#2329,.T.);
#4711=EDGE_CURVE('',#3974,#3975,#2330,.T.);
#4712=EDGE_CURVE('',#3975,#3968,#2331,.T.);
#4713=EDGE_CURVE('',#3974,#3971,#2332,.T.);
#4714=EDGE_CURVE('',#3976,#3974,#2333,.T.);
#4715=EDGE_CURVE('',#3976,#3970,#2334,.T.);
#4716=EDGE_CURVE('',#3977,#3976,#2335,.T.);
#4717=EDGE_CURVE('',#3977,#3969,#2336,.T.);
#4718=EDGE_CURVE('',#3975,#3977,#2337,.T.);
#4719=EDGE_CURVE('',#3972,#3978,#2338,.T.);
#4720=EDGE_CURVE('',#3978,#3964,#2339,.T.);
#4721=EDGE_CURVE('',#3966,#3979,#2340,.T.);
#4722=EDGE_CURVE('',#3980,#3965,#2341,.T.);
#4723=EDGE_CURVE('',#3979,#3980,#3558,.T.);
#4724=EDGE_CURVE('',#3957,#3979,#2342,.T.);
#4725=EDGE_CURVE('',#3980,#3978,#2343,.T.);
#4726=EDGE_CURVE('',#3973,#3981,#2344,.T.);
#4727=EDGE_CURVE('',#3982,#3981,#2345,.T.);
#4728=EDGE_CURVE('',#3967,#3982,#2346,.T.);
#4729=EDGE_CURVE('',#3960,#3982,#2347,.T.);
#4730=EDGE_CURVE('',#3981,#3961,#2348,.T.);
#4731=EDGE_CURVE('',#3983,#3983,#3559,.T.);
#4732=EDGE_CURVE('',#3983,#3984,#2349,.T.);
#4733=EDGE_CURVE('',#3984,#3984,#3560,.T.);
#4734=EDGE_CURVE('',#3985,#3985,#3561,.T.);
#4735=EDGE_CURVE('',#3985,#3986,#2350,.T.);
#4736=EDGE_CURVE('',#3986,#3986,#3562,.T.);
#4737=EDGE_CURVE('',#3987,#3987,#3563,.T.);
#4738=EDGE_CURVE('',#3987,#3988,#2351,.T.);
#4739=EDGE_CURVE('',#3988,#3988,#3564,.T.);
#4740=EDGE_CURVE('',#3989,#3989,#3565,.T.);
#4741=EDGE_CURVE('',#3989,#3990,#2352,.T.);
#4742=EDGE_CURVE('',#3990,#3990,#3566,.T.);
#4743=EDGE_CURVE('',#3991,#3991,#3567,.T.);
#4744=EDGE_CURVE('',#3991,#3992,#2353,.T.);
#4745=EDGE_CURVE('',#3992,#3992,#3568,.T.);
#4746=EDGE_CURVE('',#3993,#3993,#3569,.T.);
#4747=EDGE_CURVE('',#3993,#3994,#2354,.T.);
#4748=EDGE_CURVE('',#3994,#3994,#3570,.T.);
#4749=EDGE_CURVE('',#3995,#3995,#3571,.T.);
#4750=EDGE_CURVE('',#3995,#3996,#2355,.T.);
#4751=EDGE_CURVE('',#3996,#3996,#3572,.T.);
#4752=EDGE_CURVE('',#3997,#3997,#3573,.T.);
#4753=EDGE_CURVE('',#3997,#3998,#2356,.T.);
#4754=EDGE_CURVE('',#3998,#3998,#3574,.T.);
#4755=EDGE_CURVE('',#3999,#3999,#3575,.T.);
#4756=EDGE_CURVE('',#3999,#4000,#2357,.T.);
#4757=EDGE_CURVE('',#4000,#4000,#3576,.T.);
#4758=EDGE_CURVE('',#4001,#4001,#3577,.T.);
#4759=EDGE_CURVE('',#4001,#4002,#2358,.T.);
#4760=EDGE_CURVE('',#4002,#4002,#3578,.T.);
#4761=EDGE_CURVE('',#4003,#4003,#3579,.T.);
#4762=EDGE_CURVE('',#4003,#4004,#2359,.T.);
#4763=EDGE_CURVE('',#4004,#4004,#3580,.T.);
#4764=EDGE_CURVE('',#4005,#4005,#3581,.T.);
#4765=EDGE_CURVE('',#4005,#4006,#2360,.T.);
#4766=EDGE_CURVE('',#4006,#4006,#3582,.T.);
#4767=EDGE_CURVE('',#4007,#4007,#3583,.T.);
#4768=EDGE_CURVE('',#4008,#4008,#3584,.T.);
#4769=EDGE_CURVE('',#4008,#4007,#2361,.T.);
#4770=EDGE_CURVE('',#4009,#4009,#3585,.T.);
#4771=EDGE_CURVE('',#4009,#4010,#2362,.T.);
#4772=EDGE_CURVE('',#4010,#4010,#3586,.T.);
#4773=EDGE_CURVE('',#4011,#4011,#3587,.T.);
#4774=EDGE_CURVE('',#4011,#4012,#2363,.T.);
#4775=EDGE_CURVE('',#4012,#4012,#3588,.T.);
#4776=EDGE_CURVE('',#4013,#4013,#3589,.T.);
#4777=EDGE_CURVE('',#4014,#4014,#3590,.T.);
#4778=EDGE_CURVE('',#4014,#4015,#2364,.T.);
#4779=EDGE_CURVE('',#4015,#4015,#3591,.T.);
#4780=EDGE_CURVE('',#4016,#4016,#3592,.T.);
#4781=EDGE_CURVE('',#4017,#4017,#3593,.T.);
#4782=EDGE_CURVE('',#4017,#4018,#2365,.T.);
#4783=EDGE_CURVE('',#4018,#4018,#3594,.T.);
#4784=EDGE_CURVE('',#4019,#4019,#3595,.T.);
#4785=EDGE_CURVE('',#4020,#4020,#3596,.T.);
#4786=EDGE_CURVE('',#4020,#4021,#2366,.T.);
#4787=EDGE_CURVE('',#4021,#4021,#3597,.T.);
#4788=EDGE_CURVE('',#4022,#4022,#3598,.T.);
#4789=EDGE_CURVE('',#4023,#4023,#3599,.T.);
#4790=EDGE_CURVE('',#4023,#4013,#2367,.T.);
#4791=EDGE_CURVE('',#4024,#4024,#3600,.T.);
#4792=EDGE_CURVE('',#4024,#4016,#2368,.T.);
#4793=EDGE_CURVE('',#4025,#4025,#3601,.T.);
#4794=EDGE_CURVE('',#4025,#4019,#2369,.T.);
#4795=EDGE_CURVE('',#4026,#4026,#3602,.T.);
#4796=EDGE_CURVE('',#4026,#4022,#2370,.T.);
#4797=EDGE_CURVE('',#4027,#4027,#3603,.T.);
#4798=EDGE_CURVE('',#4027,#4028,#2371,.T.);
#4799=EDGE_CURVE('',#4028,#4028,#3604,.T.);
#4800=EDGE_CURVE('',#4029,#4029,#3605,.T.);
#4801=EDGE_CURVE('',#4030,#4030,#3606,.T.);
#4802=EDGE_CURVE('',#4030,#4029,#2372,.T.);
#4803=EDGE_CURVE('',#4031,#4031,#3607,.T.);
#4804=EDGE_CURVE('',#4031,#4032,#2373,.T.);
#4805=EDGE_CURVE('',#4032,#4032,#3608,.T.);
#4806=EDGE_CURVE('',#4033,#4034,#2374,.T.);
#4807=EDGE_CURVE('',#4034,#4035,#2375,.T.);
#4808=EDGE_CURVE('',#4036,#4035,#2376,.T.);
#4809=EDGE_CURVE('',#4033,#4036,#2377,.T.);
#4810=EDGE_CURVE('',#4037,#4033,#2378,.T.);
#4811=EDGE_CURVE('',#4038,#4036,#2379,.T.);
#4812=EDGE_CURVE('',#4037,#4038,#2380,.T.);
#4813=EDGE_CURVE('',#4039,#4037,#2381,.T.);
#4814=EDGE_CURVE('',#4040,#4038,#2382,.T.);
#4815=EDGE_CURVE('',#4039,#4040,#2383,.T.);
#4816=EDGE_CURVE('',#4034,#4039,#2384,.T.);
#4817=EDGE_CURVE('',#4035,#4040,#2385,.T.);
#4818=EDGE_CURVE('',#4041,#4041,#3609,.T.);
#4819=EDGE_CURVE('',#4041,#4042,#2386,.T.);
#4820=EDGE_CURVE('',#4042,#4042,#3610,.T.);
#4821=EDGE_CURVE('',#4043,#4043,#3611,.T.);
#4822=EDGE_CURVE('',#4043,#4044,#2387,.T.);
#4823=EDGE_CURVE('',#4044,#4044,#3612,.T.);
#4824=EDGE_CURVE('',#4045,#4046,#2388,.T.);
#4825=EDGE_CURVE('',#4046,#4047,#2389,.T.);
#4826=EDGE_CURVE('',#4048,#4047,#2390,.T.);
#4827=EDGE_CURVE('',#4045,#4048,#2391,.T.);
#4828=EDGE_CURVE('',#4049,#4045,#2392,.T.);
#4829=EDGE_CURVE('',#4050,#4048,#2393,.T.);
#4830=EDGE_CURVE('',#4049,#4050,#2394,.T.);
#4831=EDGE_CURVE('',#4051,#4049,#2395,.T.);
#4832=EDGE_CURVE('',#4052,#4050,#2396,.T.);
#4833=EDGE_CURVE('',#4051,#4052,#2397,.T.);
#4834=EDGE_CURVE('',#4046,#4051,#2398,.T.);
#4835=EDGE_CURVE('',#4047,#4052,#2399,.T.);
#4836=EDGE_CURVE('',#4053,#4053,#3613,.T.);
#4837=EDGE_CURVE('',#4053,#4054,#2400,.T.);
#4838=EDGE_CURVE('',#4054,#4054,#3614,.T.);
#4839=EDGE_CURVE('',#4055,#4055,#3615,.T.);
#4840=EDGE_CURVE('',#4055,#4056,#2401,.T.);
#4841=EDGE_CURVE('',#4056,#4056,#3616,.T.);
#4842=EDGE_CURVE('',#4057,#4058,#2402,.T.);
#4843=EDGE_CURVE('',#4058,#4059,#2403,.T.);
#4844=EDGE_CURVE('',#4060,#4059,#2404,.T.);
#4845=EDGE_CURVE('',#4057,#4060,#2405,.T.);
#4846=EDGE_CURVE('',#4061,#4057,#2406,.T.);
#4847=EDGE_CURVE('',#4062,#4060,#2407,.T.);
#4848=EDGE_CURVE('',#4061,#4062,#2408,.T.);
#4849=EDGE_CURVE('',#4063,#4061,#2409,.T.);
#4850=EDGE_CURVE('',#4064,#4062,#2410,.T.);
#4851=EDGE_CURVE('',#4063,#4064,#2411,.T.);
#4852=EDGE_CURVE('',#4058,#4063,#2412,.T.);
#4853=EDGE_CURVE('',#4059,#4064,#2413,.T.);
#4854=EDGE_CURVE('',#4065,#4065,#3617,.T.);
#4855=EDGE_CURVE('',#4065,#4066,#2414,.T.);
#4856=EDGE_CURVE('',#4066,#4066,#3618,.T.);
#4857=EDGE_CURVE('',#4067,#4067,#3619,.T.);
#4858=EDGE_CURVE('',#4068,#4068,#3620,.T.);
#4859=EDGE_CURVE('',#4069,#4069,#3621,.T.);
#4860=EDGE_CURVE('',#4069,#4067,#2415,.T.);
#4861=EDGE_CURVE('',#4068,#4070,#2416,.T.);
#4862=EDGE_CURVE('',#4070,#4070,#3622,.T.);
#4863=EDGE_CURVE('',#4071,#4072,#2417,.T.);
#4864=EDGE_CURVE('',#4071,#4073,#2418,.T.);
#4865=EDGE_CURVE('',#4074,#4073,#2419,.T.);
#4866=EDGE_CURVE('',#4072,#4074,#2420,.T.);
#4867=EDGE_CURVE('',#4075,#4071,#2421,.T.);
#4868=EDGE_CURVE('',#4075,#4076,#2422,.T.);
#4869=EDGE_CURVE('',#4073,#4076,#2423,.T.);
#4870=EDGE_CURVE('',#4077,#4075,#2424,.T.);
#4871=EDGE_CURVE('',#4077,#4078,#2425,.T.);
#4872=EDGE_CURVE('',#4076,#4078,#2426,.T.);
#4873=EDGE_CURVE('',#4079,#4077,#2427,.T.);
#4874=EDGE_CURVE('',#4079,#4080,#2428,.T.);
#4875=EDGE_CURVE('',#4078,#4080,#2429,.T.);
#4876=EDGE_CURVE('',#4081,#4079,#2430,.T.);
#4877=EDGE_CURVE('',#4081,#4082,#2431,.T.);
#4878=EDGE_CURVE('',#4080,#4082,#2432,.T.);
#4879=EDGE_CURVE('',#4083,#4081,#2433,.T.);
#4880=EDGE_CURVE('',#4083,#4084,#2434,.T.);
#4881=EDGE_CURVE('',#4082,#4084,#2435,.T.);
#4882=EDGE_CURVE('',#4085,#4083,#2436,.T.);
#4883=EDGE_CURVE('',#4085,#4086,#2437,.T.);
#4884=EDGE_CURVE('',#4084,#4086,#2438,.T.);
#4885=EDGE_CURVE('',#4087,#4085,#2439,.T.);
#4886=EDGE_CURVE('',#4087,#4088,#2440,.T.);
#4887=EDGE_CURVE('',#4086,#4088,#2441,.T.);
#4888=EDGE_CURVE('',#4089,#4087,#2442,.T.);
#4889=EDGE_CURVE('',#4090,#4089,#2443,.T.);
#4890=EDGE_CURVE('',#4088,#4090,#2444,.T.);
#4891=EDGE_CURVE('',#4091,#4092,#2445,.T.);
#4892=EDGE_CURVE('',#4091,#4093,#2446,.T.);
#4893=EDGE_CURVE('',#4094,#4093,#2447,.T.);
#4894=EDGE_CURVE('',#4092,#4094,#2448,.T.);
#4895=EDGE_CURVE('',#4095,#4091,#2449,.T.);
#4896=EDGE_CURVE('',#4095,#4096,#2450,.T.);
#4897=EDGE_CURVE('',#4093,#4096,#2451,.T.);
#4898=EDGE_CURVE('',#4097,#4095,#2452,.T.);
#4899=EDGE_CURVE('',#4097,#4098,#2453,.T.);
#4900=EDGE_CURVE('',#4096,#4098,#2454,.T.);
#4901=EDGE_CURVE('',#4099,#4097,#2455,.T.);
#4902=EDGE_CURVE('',#4099,#4100,#2456,.T.);
#4903=EDGE_CURVE('',#4098,#4100,#2457,.T.);
#4904=EDGE_CURVE('',#4101,#4099,#2458,.T.);
#4905=EDGE_CURVE('',#4101,#4102,#2459,.T.);
#4906=EDGE_CURVE('',#4100,#4102,#2460,.T.);
#4907=EDGE_CURVE('',#4103,#4101,#2461,.T.);
#4908=EDGE_CURVE('',#4103,#4104,#2462,.T.);
#4909=EDGE_CURVE('',#4102,#4104,#2463,.T.);
#4910=EDGE_CURVE('',#4105,#4103,#2464,.T.);
#4911=EDGE_CURVE('',#4105,#4106,#2465,.T.);
#4912=EDGE_CURVE('',#4104,#4106,#2466,.T.);
#4913=EDGE_CURVE('',#4107,#4105,#2467,.T.);
#4914=EDGE_CURVE('',#4107,#4108,#2468,.T.);
#4915=EDGE_CURVE('',#4106,#4108,#2469,.T.);
#4916=EDGE_CURVE('',#4109,#4107,#2470,.T.);
#4917=EDGE_CURVE('',#4110,#4109,#2471,.T.);
#4918=EDGE_CURVE('',#4108,#4110,#2472,.T.);
#4919=EDGE_CURVE('',#4111,#4112,#2473,.T.);
#4920=EDGE_CURVE('',#4111,#4113,#2474,.T.);
#4921=EDGE_CURVE('',#4114,#4113,#2475,.T.);
#4922=EDGE_CURVE('',#4112,#4114,#2476,.T.);
#4923=EDGE_CURVE('',#4115,#4111,#2477,.T.);
#4924=EDGE_CURVE('',#4115,#4116,#2478,.T.);
#4925=EDGE_CURVE('',#4113,#4116,#2479,.T.);
#4926=EDGE_CURVE('',#4117,#4115,#2480,.T.);
#4927=EDGE_CURVE('',#4117,#4118,#2481,.T.);
#4928=EDGE_CURVE('',#4116,#4118,#2482,.T.);
#4929=EDGE_CURVE('',#4119,#4117,#2483,.T.);
#4930=EDGE_CURVE('',#4119,#4120,#2484,.T.);
#4931=EDGE_CURVE('',#4118,#4120,#2485,.T.);
#4932=EDGE_CURVE('',#4121,#4119,#2486,.T.);
#4933=EDGE_CURVE('',#4121,#4122,#2487,.T.);
#4934=EDGE_CURVE('',#4120,#4122,#2488,.T.);
#4935=EDGE_CURVE('',#4123,#4121,#2489,.T.);
#4936=EDGE_CURVE('',#4123,#4124,#2490,.T.);
#4937=EDGE_CURVE('',#4122,#4124,#2491,.T.);
#4938=EDGE_CURVE('',#4125,#4123,#2492,.T.);
#4939=EDGE_CURVE('',#4125,#4126,#2493,.T.);
#4940=EDGE_CURVE('',#4124,#4126,#2494,.T.);
#4941=EDGE_CURVE('',#4127,#4125,#2495,.T.);
#4942=EDGE_CURVE('',#4127,#4128,#2496,.T.);
#4943=EDGE_CURVE('',#4126,#4128,#2497,.T.);
#4944=EDGE_CURVE('',#4129,#4127,#2498,.T.);
#4945=EDGE_CURVE('',#4130,#4129,#2499,.T.);
#4946=EDGE_CURVE('',#4128,#4130,#2500,.T.);
#4947=EDGE_CURVE('',#4131,#4132,#2501,.T.);
#4948=EDGE_CURVE('',#4131,#4133,#2502,.T.);
#4949=EDGE_CURVE('',#4134,#4133,#2503,.T.);
#4950=EDGE_CURVE('',#4132,#4134,#2504,.T.);
#4951=EDGE_CURVE('',#4135,#4131,#2505,.T.);
#4952=EDGE_CURVE('',#4135,#4136,#2506,.T.);
#4953=EDGE_CURVE('',#4133,#4136,#2507,.T.);
#4954=EDGE_CURVE('',#4137,#4135,#2508,.T.);
#4955=EDGE_CURVE('',#4137,#4138,#2509,.T.);
#4956=EDGE_CURVE('',#4136,#4138,#2510,.T.);
#4957=EDGE_CURVE('',#4139,#4137,#2511,.T.);
#4958=EDGE_CURVE('',#4139,#4140,#2512,.T.);
#4959=EDGE_CURVE('',#4138,#4140,#2513,.T.);
#4960=EDGE_CURVE('',#4141,#4139,#2514,.T.);
#4961=EDGE_CURVE('',#4141,#4142,#2515,.T.);
#4962=EDGE_CURVE('',#4140,#4142,#2516,.T.);
#4963=EDGE_CURVE('',#4143,#4141,#2517,.T.);
#4964=EDGE_CURVE('',#4143,#4144,#2518,.T.);
#4965=EDGE_CURVE('',#4142,#4144,#2519,.T.);
#4966=EDGE_CURVE('',#4145,#4143,#2520,.T.);
#4967=EDGE_CURVE('',#4145,#4146,#2521,.T.);
#4968=EDGE_CURVE('',#4144,#4146,#2522,.T.);
#4969=EDGE_CURVE('',#4147,#4145,#2523,.T.);
#4970=EDGE_CURVE('',#4147,#4148,#2524,.T.);
#4971=EDGE_CURVE('',#4146,#4148,#2525,.T.);
#4972=EDGE_CURVE('',#4149,#4147,#2526,.T.);
#4973=EDGE_CURVE('',#4150,#4149,#2527,.T.);
#4974=EDGE_CURVE('',#4148,#4150,#2528,.T.);
#4975=EDGE_CURVE('',#4151,#4151,#3623,.T.);
#4976=EDGE_CURVE('',#4151,#4152,#2529,.T.);
#4977=EDGE_CURVE('',#4152,#4152,#3624,.T.);
#4978=EDGE_CURVE('',#4089,#4153,#2530,.T.);
#4979=EDGE_CURVE('',#4153,#4154,#2531,.T.);
#4980=EDGE_CURVE('',#4090,#4154,#2532,.T.);
#4981=EDGE_CURVE('',#4155,#4074,#2533,.T.);
#4982=EDGE_CURVE('',#4156,#4155,#2534,.T.);
#4983=EDGE_CURVE('',#4156,#4072,#2535,.T.);
#4984=EDGE_CURVE('',#4109,#4156,#2536,.T.);
#4985=EDGE_CURVE('',#4110,#4155,#2537,.T.);
#4986=EDGE_CURVE('',#4157,#4094,#2538,.T.);
#4987=EDGE_CURVE('',#4158,#4157,#2539,.T.);
#4988=EDGE_CURVE('',#4158,#4092,#2540,.T.);
#4989=EDGE_CURVE('',#4129,#4158,#2541,.T.);
#4990=EDGE_CURVE('',#4130,#4157,#2542,.T.);
#4991=EDGE_CURVE('',#4159,#4114,#2543,.T.);
#4992=EDGE_CURVE('',#4160,#4159,#2544,.T.);
#4993=EDGE_CURVE('',#4160,#4112,#2545,.T.);
#4994=EDGE_CURVE('',#4149,#4160,#2546,.T.);
#4995=EDGE_CURVE('',#4150,#4159,#2547,.T.);
#4996=EDGE_CURVE('',#4154,#4134,#2548,.T.);
#4997=EDGE_CURVE('',#4153,#4132,#2549,.T.);
#4998=EDGE_CURVE('',#4161,#4162,#2550,.T.);
#4999=EDGE_CURVE('',#4163,#4161,#2551,.T.);
#5000=EDGE_CURVE('',#4164,#4163,#2552,.T.);
#5001=EDGE_CURVE('',#4162,#4164,#2553,.T.);
#5002=EDGE_CURVE('',#4163,#4165,#2554,.T.);
#5003=EDGE_CURVE('',#4166,#4165,#2555,.T.);
#5004=EDGE_CURVE('',#4164,#4166,#2556,.T.);
#5005=EDGE_CURVE('',#4165,#4167,#2557,.T.);
#5006=EDGE_CURVE('',#4167,#4168,#2558,.T.);
#5007=EDGE_CURVE('',#4168,#4166,#2559,.T.);
#5008=EDGE_CURVE('',#4169,#4169,#3625,.T.);
#5009=EDGE_CURVE('',#4170,#4161,#2560,.T.);
#5010=EDGE_CURVE('',#4171,#4170,#2561,.T.);
#5011=EDGE_CURVE('',#4171,#4172,#2562,.T.);
#5012=EDGE_CURVE('',#4173,#4172,#2563,.T.);
#5013=EDGE_CURVE('',#4173,#4174,#2564,.T.);
#5014=EDGE_CURVE('',#4174,#4175,#2565,.T.);
#5015=EDGE_CURVE('',#4175,#4167,#2566,.T.);
#5016=EDGE_CURVE('',#4175,#4176,#2567,.T.);
#5017=EDGE_CURVE('',#4176,#4168,#2568,.T.);
#5018=EDGE_CURVE('',#4177,#4174,#2569,.T.);
#5019=EDGE_CURVE('',#4176,#4177,#2570,.T.);
#5020=EDGE_CURVE('',#4178,#4177,#2571,.T.);
#5021=EDGE_CURVE('',#4179,#4178,#2572,.T.);
#5022=EDGE_CURVE('',#4179,#4180,#2573,.T.);
#5023=EDGE_CURVE('',#4181,#4180,#2574,.T.);
#5024=EDGE_CURVE('',#4181,#4162,#2575,.T.);
#5025=EDGE_CURVE('',#4178,#4173,#2576,.T.);
#5026=EDGE_CURVE('',#4172,#4182,#2577,.T.);
#5027=EDGE_CURVE('',#4182,#4183,#427,.T.);
#5028=EDGE_CURVE('',#4183,#4179,#2578,.T.);
#5029=EDGE_CURVE('',#4184,#4182,#3626,.F.);
#5030=EDGE_CURVE('',#4184,#4169,#2579,.T.);
#5031=EDGE_CURVE('',#4185,#4184,#3627,.F.);
#5032=EDGE_CURVE('',#4186,#4185,#428,.T.);
#5033=EDGE_CURVE('',#4183,#4186,#3628,.F.);
#5034=EDGE_CURVE('',#4185,#4171,#2580,.T.);
#5035=EDGE_CURVE('',#4180,#4186,#2581,.T.);
#5036=EDGE_CURVE('',#4170,#4181,#2582,.T.);
#5037=EDGE_CURVE('',#4187,#4187,#3629,.T.);
#5038=EDGE_CURVE('',#4187,#4188,#2583,.T.);
#5039=EDGE_CURVE('',#4188,#4188,#3630,.T.);
#5040=EDGE_CURVE('',#4188,#4189,#2584,.T.);
#5041=EDGE_CURVE('',#4189,#4189,#3631,.T.);
#5042=EDGE_CURVE('',#4190,#4190,#3632,.T.);
#5043=EDGE_CURVE('',#4190,#4191,#2585,.T.);
#5044=EDGE_CURVE('',#4191,#4191,#3633,.T.);
#5045=EDGE_CURVE('',#4192,#4193,#2586,.T.);
#5046=EDGE_CURVE('',#4193,#4194,#2587,.T.);
#5047=EDGE_CURVE('',#4194,#4195,#2588,.T.);
#5048=EDGE_CURVE('',#4192,#4195,#2589,.T.);
#5049=EDGE_CURVE('',#4193,#4196,#2590,.T.);
#5050=EDGE_CURVE('',#4196,#4197,#2591,.T.);
#5051=EDGE_CURVE('',#4197,#4194,#2592,.T.);
#5052=EDGE_CURVE('',#4196,#4198,#2593,.T.);
#5053=EDGE_CURVE('',#4198,#4199,#2594,.T.);
#5054=EDGE_CURVE('',#4199,#4197,#2595,.T.);
#5055=EDGE_CURVE('',#4198,#4200,#2596,.T.);
#5056=EDGE_CURVE('',#4200,#4201,#2597,.T.);
#5057=EDGE_CURVE('',#4201,#4199,#2598,.T.);
#5058=EDGE_CURVE('',#4200,#4202,#2599,.T.);
#5059=EDGE_CURVE('',#4202,#4203,#2600,.T.);
#5060=EDGE_CURVE('',#4203,#4201,#2601,.T.);
#5061=EDGE_CURVE('',#4202,#4192,#2602,.T.);
#5062=EDGE_CURVE('',#4195,#4203,#2603,.T.);
#5063=EDGE_CURVE('',#4204,#4204,#3634,.T.);
#5064=EDGE_CURVE('',#4205,#4205,#3635,.T.);
#5065=EDGE_CURVE('',#4206,#4206,#3636,.T.);
#5066=EDGE_CURVE('',#4206,#4205,#2604,.T.);
#5067=EDGE_CURVE('',#4207,#4207,#3637,.T.);
#5068=EDGE_CURVE('',#4207,#4206,#2605,.T.);
#5069=EDGE_CURVE('',#4208,#4208,#3638,.T.);
#5070=EDGE_CURVE('',#4208,#4207,#2606,.T.);
#5071=EDGE_CURVE('',#4209,#4209,#3639,.T.);
#5072=EDGE_CURVE('',#4210,#4210,#3640,.F.);
#5073=EDGE_CURVE('',#4210,#4209,#2607,.T.);
#5074=EDGE_CURVE('',#4204,#4210,#2608,.T.);
#5075=EDGE_CURVE('',#4211,#4212,#3641,.T.);
#5076=EDGE_CURVE('',#4212,#4211,#3642,.T.);
#5077=EDGE_CURVE('',#4212,#4213,#3643,.T.);
#5078=EDGE_CURVE('',#4214,#4213,#3644,.T.);
#5079=EDGE_CURVE('',#4213,#4214,#3645,.T.);
#5080=EDGE_CURVE('',#4214,#4215,#2609,.T.);
#5081=EDGE_CURVE('',#4215,#4215,#3646,.T.);
#5082=EDGE_CURVE('',#4216,#4216,#3647,.T.);
#5083=EDGE_CURVE('',#4216,#4217,#2610,.T.);
#5084=EDGE_CURVE('',#4217,#4217,#3648,.T.);
#5085=EDGE_CURVE('',#4217,#4218,#2611,.T.);
#5086=EDGE_CURVE('',#4218,#4218,#3649,.T.);
#5087=EDGE_CURVE('',#4219,#4219,#3650,.T.);
#5088=EDGE_CURVE('',#4219,#4211,#2612,.T.);
#5089=EDGE_CURVE('',#4220,#4220,#3651,.T.);
#5090=EDGE_CURVE('',#4220,#4216,#2613,.T.);
#5091=EDGE_CURVE('',#4221,#4222,#3652,.T.);
#5092=EDGE_CURVE('',#4222,#4221,#3653,.T.);
#5093=EDGE_CURVE('',#4222,#4223,#3654,.T.);
#5094=EDGE_CURVE('',#4224,#4223,#3655,.T.);
#5095=EDGE_CURVE('',#4223,#4224,#3656,.T.);
#5096=EDGE_CURVE('',#4225,#4225,#3657,.T.);
#5097=EDGE_CURVE('',#4225,#4224,#2614,.T.);
#5098=EDGE_CURVE('',#4226,#4226,#3658,.T.);
#5099=EDGE_CURVE('',#4227,#4227,#3659,.T.);
#5100=EDGE_CURVE('',#4228,#4228,#3660,.T.);
#5101=EDGE_CURVE('',#4228,#4226,#2615,.T.);
#5102=EDGE_CURVE('',#4229,#4229,#3661,.T.);
#5103=EDGE_CURVE('',#4229,#4228,#2616,.T.);
#5104=EDGE_CURVE('',#4230,#4230,#3662,.T.);
#5105=EDGE_CURVE('',#4230,#4229,#2617,.T.);
#5106=EDGE_CURVE('',#4221,#4227,#2618,.T.);
#5107=EDGE_CURVE('',#4231,#4232,#3663,.T.);
#5108=EDGE_CURVE('',#4233,#4234,#3664,.T.);
#5109=EDGE_CURVE('',#4235,#4236,#3665,.T.);
#5110=EDGE_CURVE('',#4237,#4238,#3666,.T.);
#5111=EDGE_CURVE('',#4239,#4240,#3667,.T.);
#5112=EDGE_CURVE('',#4241,#4242,#3668,.T.);
#5113=EDGE_CURVE('',#4243,#4244,#3669,.T.);
#5114=EDGE_CURVE('',#4245,#4246,#3670,.T.);
#5115=EDGE_CURVE('',#4247,#4248,#355,.T.);
#5116=EDGE_CURVE('',#4249,#4247,#3671,.T.);
#5117=EDGE_CURVE('',#4250,#4249,#356,.T.);
#5118=EDGE_CURVE('',#4248,#4250,#3672,.T.);
#5119=EDGE_CURVE('',#4251,#4249,#3673,.T.);
#5120=EDGE_CURVE('',#4251,#4252,#357,.T.);
#5121=EDGE_CURVE('',#4253,#4252,#3674,.T.);
#5122=EDGE_CURVE('',#4253,#4254,#358,.T.);
#5123=EDGE_CURVE('',#4255,#4254,#3675,.T.);
#5124=EDGE_CURVE('',#4255,#4256,#359,.T.);
#5125=EDGE_CURVE('',#4256,#4257,#2619,.T.);
#5126=EDGE_CURVE('',#4257,#4257,#3676,.T.);
#5127=EDGE_CURVE('',#4256,#4258,#360,.T.);
#5128=EDGE_CURVE('',#4259,#4258,#3677,.T.);
#5129=EDGE_CURVE('',#4259,#4260,#361,.T.);
#5130=EDGE_CURVE('',#4261,#4260,#3678,.T.);
#5131=EDGE_CURVE('',#4261,#4262,#362,.T.);
#5132=EDGE_CURVE('',#4263,#4262,#3679,.T.);
#5133=EDGE_CURVE('',#4263,#4264,#363,.T.);
#5134=EDGE_CURVE('',#4265,#4264,#3680,.T.);
#5135=EDGE_CURVE('',#4265,#4266,#364,.T.);
#5136=EDGE_CURVE('',#4250,#4266,#3681,.T.);
#5137=EDGE_CURVE('',#4247,#4267,#3682,.T.);
#5138=EDGE_CURVE('',#4267,#4251,#3683,.T.);
#5139=EDGE_CURVE('',#4268,#4267,#365,.T.);
#5140=EDGE_CURVE('',#4252,#4268,#3684,.T.);
#5141=EDGE_CURVE('',#4268,#4269,#3685,.T.);
#5142=EDGE_CURVE('',#4269,#4253,#3686,.T.);
#5143=EDGE_CURVE('',#4270,#4269,#366,.T.);
#5144=EDGE_CURVE('',#4254,#4270,#3687,.T.);
#5145=EDGE_CURVE('',#4270,#4271,#3688,.T.);
#5146=EDGE_CURVE('',#4271,#4255,#3689,.T.);
#5147=EDGE_CURVE('',#4272,#4273,#367,.T.);
#5148=EDGE_CURVE('',#4258,#4272,#3690,.T.);
#5149=EDGE_CURVE('',#4273,#4271,#368,.T.);
#5150=EDGE_CURVE('',#4272,#4274,#3691,.T.);
#5151=EDGE_CURVE('',#4274,#4259,#3692,.T.);
#5152=EDGE_CURVE('',#4275,#4274,#369,.T.);
#5153=EDGE_CURVE('',#4260,#4275,#3693,.T.);
#5154=EDGE_CURVE('',#4275,#4276,#3694,.T.);
#5155=EDGE_CURVE('',#4276,#4261,#3695,.T.);
#5156=EDGE_CURVE('',#4277,#4276,#370,.T.);
#5157=EDGE_CURVE('',#4262,#4277,#3696,.T.);
#5158=EDGE_CURVE('',#4277,#4278,#3697,.T.);
#5159=EDGE_CURVE('',#4278,#4263,#3698,.T.);
#5160=EDGE_CURVE('',#4279,#4278,#371,.T.);
#5161=EDGE_CURVE('',#4264,#4279,#3699,.T.);
#5162=EDGE_CURVE('',#4280,#4280,#3700,.T.);
#5163=EDGE_CURVE('',#4280,#4273,#2620,.T.);
#5164=EDGE_CURVE('',#4281,#4248,#3701,.T.);
#5165=EDGE_CURVE('',#4281,#4282,#372,.T.);
#5166=EDGE_CURVE('',#4279,#4282,#3702,.T.);
#5167=EDGE_CURVE('',#4266,#4281,#3703,.T.);
#5168=EDGE_CURVE('',#4282,#4265,#3704,.T.);
#5169=EDGE_CURVE('',#4283,#4283,#3705,.T.);
#5170=EDGE_CURVE('',#4284,#4284,#3706,.T.);
#5171=EDGE_CURVE('',#4285,#4285,#3707,.T.);
#5172=EDGE_CURVE('',#4285,#4283,#2621,.T.);
#5173=EDGE_CURVE('',#4286,#4286,#3708,.T.);
#5174=EDGE_CURVE('',#4286,#4284,#2622,.T.);
#5175=EDGE_CURVE('',#4287,#4287,#3709,.T.);
#5176=EDGE_CURVE('',#4288,#4288,#3710,.T.);
#5177=EDGE_CURVE('',#4289,#4289,#3711,.T.);
#5178=EDGE_CURVE('',#4289,#4287,#2623,.T.);
#5179=EDGE_CURVE('',#4290,#4290,#3712,.T.);
#5180=EDGE_CURVE('',#4290,#4288,#2624,.T.);
#5181=EDGE_CURVE('',#4291,#4292,#3713,.T.);
#5182=EDGE_CURVE('',#4293,#4291,#2625,.T.);
#5183=EDGE_CURVE('',#4294,#4293,#2626,.T.);
#5184=EDGE_CURVE('',#4292,#4294,#2627,.T.);
#5185=EDGE_CURVE('',#4292,#4295,#2628,.T.);
#5186=EDGE_CURVE('',#4296,#4294,#2629,.T.);
#5187=EDGE_CURVE('',#4296,#4295,#2630,.T.);
#5188=EDGE_CURVE('',#4295,#4297,#3714,.T.);
#5189=EDGE_CURVE('',#4298,#4296,#2631,.T.);
#5190=EDGE_CURVE('',#4297,#4298,#2632,.T.);
#5191=EDGE_CURVE('',#4297,#4291,#2633,.T.);
#5192=EDGE_CURVE('',#4298,#4293,#2634,.T.);
#5193=EDGE_CURVE('',#4299,#4299,#3715,.T.);
#5194=EDGE_CURVE('',#4300,#4300,#3716,.T.);
#5195=EDGE_CURVE('',#4301,#4301,#3717,.T.);
#5196=EDGE_CURVE('',#4301,#4299,#2635,.T.);
#5197=EDGE_CURVE('',#4302,#4302,#3718,.T.);
#5198=EDGE_CURVE('',#4303,#4303,#3719,.T.);
#5199=EDGE_CURVE('',#4303,#4302,#2636,.T.);
#5200=EDGE_CURVE('',#4304,#4304,#3720,.T.);
#5201=EDGE_CURVE('',#4305,#4305,#3721,.T.);
#5202=EDGE_CURVE('',#4305,#4304,#2637,.T.);
#5203=EDGE_CURVE('',#4306,#4306,#3722,.T.);
#5204=EDGE_CURVE('',#4307,#4307,#3723,.T.);
#5205=EDGE_CURVE('',#4307,#4306,#2638,.T.);
#5206=EDGE_CURVE('',#4308,#4308,#3724,.T.);
#5207=EDGE_CURVE('',#4309,#4309,#3725,.T.);
#5208=EDGE_CURVE('',#4309,#4308,#2639,.T.);
#5209=EDGE_CURVE('',#4310,#4310,#3726,.T.);
#5210=EDGE_CURVE('',#4310,#4300,#2640,.T.);
#5211=EDGE_CURVE('',#4311,#4312,#3727,.T.);
#5212=EDGE_CURVE('',#4313,#4311,#2641,.T.);
#5213=EDGE_CURVE('',#4314,#4313,#3728,.T.);
#5214=EDGE_CURVE('',#4312,#4314,#2642,.T.);
#5215=EDGE_CURVE('',#4312,#4315,#2643,.T.);
#5216=EDGE_CURVE('',#4316,#4314,#2644,.T.);
#5217=EDGE_CURVE('',#4316,#4315,#2645,.T.);
#5218=EDGE_CURVE('',#4315,#4317,#3729,.T.);
#5219=EDGE_CURVE('',#4318,#4316,#3730,.T.);
#5220=EDGE_CURVE('',#4317,#4318,#2646,.T.);
#5221=EDGE_CURVE('',#4317,#4311,#2647,.T.);
#5222=EDGE_CURVE('',#4313,#4318,#2648,.T.);
#5223=EDGE_CURVE('',#4319,#4319,#3731,.T.);
#5224=EDGE_CURVE('',#4320,#4320,#3732,.T.);
#5225=EDGE_CURVE('',#4321,#4321,#3733,.T.);
#5226=EDGE_CURVE('',#4321,#4319,#2649,.T.);
#5227=EDGE_CURVE('',#4322,#4322,#3734,.T.);
#5228=EDGE_CURVE('',#4322,#4320,#2650,.T.);
#5229=EDGE_CURVE('',#4323,#4324,#2651,.T.);
#5230=EDGE_CURVE('',#4324,#4325,#2652,.T.);
#5231=EDGE_CURVE('',#4325,#4326,#2653,.T.);
#5232=EDGE_CURVE('',#4323,#4326,#2654,.T.);
#5233=EDGE_CURVE('',#4324,#4327,#2655,.T.);
#5234=EDGE_CURVE('',#4327,#4328,#2656,.T.);
#5235=EDGE_CURVE('',#4328,#4325,#2657,.T.);
#5236=EDGE_CURVE('',#4327,#4329,#2658,.T.);
#5237=EDGE_CURVE('',#4329,#4330,#2659,.T.);
#5238=EDGE_CURVE('',#4330,#4328,#2660,.T.);
#5239=EDGE_CURVE('',#4329,#4331,#2661,.T.);
#5240=EDGE_CURVE('',#4331,#4332,#2662,.T.);
#5241=EDGE_CURVE('',#4332,#4330,#2663,.T.);
#5242=EDGE_CURVE('',#4331,#4333,#2664,.T.);
#5243=EDGE_CURVE('',#4333,#4334,#2665,.T.);
#5244=EDGE_CURVE('',#4334,#4332,#2666,.T.);
#5245=EDGE_CURVE('',#4333,#4323,#2667,.T.);
#5246=EDGE_CURVE('',#4326,#4334,#2668,.T.);
#5247=EDGE_CURVE('',#4335,#4335,#3735,.T.);
#5248=EDGE_CURVE('',#4336,#4336,#3736,.T.);
#5249=EDGE_CURVE('',#4335,#4337,#2669,.T.);
#5250=EDGE_CURVE('',#4337,#4337,#3737,.T.);
#5251=EDGE_CURVE('',#4338,#4338,#3738,.T.);
#5252=EDGE_CURVE('',#4339,#4339,#3739,.T.);
#5253=EDGE_CURVE('',#4339,#4338,#2670,.T.);
#5254=EDGE_CURVE('',#4340,#4340,#3740,.T.);
#5255=EDGE_CURVE('',#4340,#4339,#2671,.T.);
#5256=EDGE_CURVE('',#4341,#4341,#3741,.T.);
#5257=EDGE_CURVE('',#4341,#4340,#2672,.T.);
#5258=EDGE_CURVE('',#4342,#4342,#3742,.T.);
#5259=EDGE_CURVE('',#4343,#4343,#3743,.F.);
#5260=EDGE_CURVE('',#4343,#4342,#2673,.T.);
#5261=EDGE_CURVE('',#4344,#4344,#3744,.F.);
#5262=EDGE_CURVE('',#4344,#4343,#2674,.T.);
#5263=EDGE_CURVE('',#4336,#4344,#2675,.T.);
#5264=EDGE_CURVE('',#4345,#4345,#3745,.T.);
#5265=EDGE_CURVE('',#4345,#4346,#2676,.T.);
#5266=EDGE_CURVE('',#4346,#4346,#3746,.T.);
#5267=EDGE_CURVE('',#4347,#4348,#2677,.T.);
#5268=EDGE_CURVE('',#4349,#4347,#3747,.T.);
#5269=EDGE_CURVE('',#4350,#4349,#2678,.T.);
#5270=EDGE_CURVE('',#4350,#4348,#3748,.T.);
#5271=EDGE_CURVE('',#4351,#4350,#2679,.T.);
#5272=EDGE_CURVE('',#4352,#4351,#3749,.T.);
#5273=EDGE_CURVE('',#4353,#4352,#3750,.T.);
#5274=EDGE_CURVE('',#4354,#4353,#2680,.T.);
#5275=EDGE_CURVE('',#4355,#4354,#3751,.T.);
#5276=EDGE_CURVE('',#4356,#4355,#2681,.T.);
#5277=EDGE_CURVE('',#4357,#4356,#3752,.T.);
#5278=EDGE_CURVE('',#4348,#4357,#2682,.T.);
#5279=EDGE_CURVE('',#4358,#4358,#3753,.T.);
#5280=EDGE_CURVE('',#4359,#4349,#2683,.T.);
#5281=EDGE_CURVE('',#4351,#4359,#2684,.T.);
#5282=EDGE_CURVE('',#4347,#4360,#2685,.T.);
#5283=EDGE_CURVE('',#4359,#4360,#3754,.T.);
#5284=EDGE_CURVE('',#4360,#4357,#2686,.T.);
#5285=EDGE_CURVE('',#4361,#4354,#2687,.T.);
#5286=EDGE_CURVE('',#4362,#4361,#3755,.T.);
#5287=EDGE_CURVE('',#4355,#4362,#2688,.T.);
#5288=EDGE_CURVE('',#4363,#4362,#2689,.T.);
#5289=EDGE_CURVE('',#4356,#4363,#2690,.T.);
#5290=EDGE_CURVE('',#4361,#4364,#2691,.T.);
#5291=EDGE_CURVE('',#4363,#4364,#3756,.T.);
#5292=EDGE_CURVE('',#4364,#4353,#2692,.T.);
#5293=EDGE_CURVE('',#4365,#4365,#3757,.T.);
#5294=EDGE_CURVE('',#4366,#4366,#3758,.T.);
#5295=EDGE_CURVE('',#4365,#4352,#2693,.T.);
#5296=EDGE_CURVE('',#4367,#4367,#3759,.T.);
#5297=EDGE_CURVE('',#4368,#4368,#3760,.T.);
#5298=EDGE_CURVE('',#4367,#4366,#2694,.T.);
#5299=EDGE_CURVE('',#4358,#4369,#2695,.T.);
#5300=EDGE_CURVE('',#4369,#4369,#3761,.T.);
#5301=EDGE_CURVE('',#4370,#4370,#3762,.T.);
#5302=EDGE_CURVE('',#4370,#4368,#2696,.T.);
#5303=EDGE_CURVE('',#4371,#4371,#3763,.T.);
#5304=EDGE_CURVE('',#4371,#4372,#2697,.T.);
#5305=EDGE_CURVE('',#4372,#4372,#3764,.T.);
#5306=EDGE_CURVE('',#4373,#4373,#3765,.T.);
#5307=EDGE_CURVE('',#4373,#4374,#2698,.T.);
#5308=EDGE_CURVE('',#4374,#4374,#3766,.T.);
#5309=EDGE_CURVE('',#4375,#4376,#2699,.T.);
#5310=EDGE_CURVE('',#4375,#4376,#3767,.T.);
#5311=EDGE_CURVE('',#4377,#4375,#373,.T.);
#5312=EDGE_CURVE('',#4378,#4377,#3768,.T.);
#5313=EDGE_CURVE('',#4378,#4379,#2700,.T.);
#5314=EDGE_CURVE('',#4380,#4379,#374,.T.);
#5315=EDGE_CURVE('',#4379,#4380,#375,.T.);
#5316=EDGE_CURVE('',#4381,#4378,#3769,.T.);
#5317=EDGE_CURVE('',#4376,#4381,#376,.T.);
#5318=EDGE_CURVE('',#4381,#4377,#2701,.T.);
#5319=EDGE_CURVE('',#4382,#4382,#3770,.T.);
#5320=EDGE_CURVE('',#4382,#4383,#2702,.T.);
#5321=EDGE_CURVE('',#4383,#4383,#3771,.T.);
#5322=EDGE_CURVE('',#4384,#4384,#3772,.T.);
#5323=EDGE_CURVE('',#4384,#4385,#2703,.T.);
#5324=EDGE_CURVE('',#4385,#4385,#3773,.T.);
#5325=EDGE_CURVE('',#4386,#4386,#3774,.T.);
#5326=EDGE_CURVE('',#4386,#4387,#2704,.T.);
#5327=EDGE_CURVE('',#4387,#4387,#3775,.T.);
#5328=EDGE_CURVE('',#4388,#4388,#3776,.T.);
#5329=EDGE_CURVE('',#4388,#4389,#2705,.T.);
#5330=EDGE_CURVE('',#4389,#4389,#3777,.T.);
#5331=EDGE_CURVE('',#4390,#4390,#3778,.T.);
#5332=EDGE_CURVE('',#4391,#4391,#3779,.T.);
#5333=EDGE_CURVE('',#4392,#4392,#3780,.T.);
#5334=EDGE_CURVE('',#4393,#4393,#3781,.T.);
#5335=EDGE_CURVE('',#4390,#4392,#2706,.T.);
#5336=EDGE_CURVE('',#4393,#4394,#2707,.T.);
#5337=EDGE_CURVE('',#4394,#4394,#3782,.T.);
#5338=EDGE_CURVE('',#4395,#4395,#3783,.T.);
#5339=EDGE_CURVE('',#4395,#4391,#2708,.T.);
#5340=EDGE_CURVE('',#4396,#4396,#3784,.T.);
#5341=EDGE_CURVE('',#4396,#4397,#2709,.T.);
#5342=EDGE_CURVE('',#4397,#4397,#3785,.T.);
#5343=EDGE_CURVE('',#4398,#4398,#3786,.T.);
#5344=EDGE_CURVE('',#4398,#4399,#2710,.T.);
#5345=EDGE_CURVE('',#4399,#4399,#3787,.T.);
#5346=EDGE_CURVE('',#4400,#4400,#3788,.T.);
#5347=EDGE_CURVE('',#4400,#4401,#2711,.T.);
#5348=EDGE_CURVE('',#4401,#4401,#3789,.T.);
#5349=EDGE_CURVE('',#4402,#4402,#3790,.T.);
#5350=EDGE_CURVE('',#4402,#4403,#2712,.T.);
#5351=EDGE_CURVE('',#4403,#4403,#3791,.T.);
#5352=EDGE_CURVE('',#4404,#4404,#3792,.T.);
#5353=EDGE_CURVE('',#4404,#4405,#2713,.T.);
#5354=EDGE_CURVE('',#4405,#4405,#3793,.T.);
#5355=EDGE_CURVE('',#4406,#4406,#3794,.T.);
#5356=EDGE_CURVE('',#4406,#4407,#2714,.T.);
#5357=EDGE_CURVE('',#4407,#4407,#3795,.T.);
#5358=EDGE_CURVE('',#4408,#4408,#3796,.T.);
#5359=EDGE_CURVE('',#4408,#4409,#2715,.T.);
#5360=EDGE_CURVE('',#4409,#4409,#3797,.T.);
#5361=EDGE_CURVE('',#4410,#4410,#3798,.T.);
#5362=EDGE_CURVE('',#4410,#4411,#2716,.T.);
#5363=EDGE_CURVE('',#4411,#4411,#3799,.T.);
#5364=EDGE_CURVE('',#4412,#4412,#3800,.T.);
#5365=EDGE_CURVE('',#4413,#4414,#2717,.T.);
#5366=EDGE_CURVE('',#4413,#4415,#2718,.T.);
#5367=EDGE_CURVE('',#4415,#4416,#2719,.T.);
#5368=EDGE_CURVE('',#4414,#4416,#2720,.T.);
#5369=EDGE_CURVE('',#4417,#4413,#2721,.T.);
#5370=EDGE_CURVE('',#4417,#4418,#2722,.T.);
#5371=EDGE_CURVE('',#4418,#4415,#2723,.T.);
#5372=EDGE_CURVE('',#4419,#4417,#2724,.T.);
#5373=EDGE_CURVE('',#4419,#4420,#2725,.T.);
#5374=EDGE_CURVE('',#4420,#4418,#2726,.T.);
#5375=EDGE_CURVE('',#4421,#4419,#2727,.T.);
#5376=EDGE_CURVE('',#4421,#4422,#2728,.T.);
#5377=EDGE_CURVE('',#4422,#4420,#2729,.T.);
#5378=EDGE_CURVE('',#4423,#4421,#2730,.T.);
#5379=EDGE_CURVE('',#4423,#4424,#2731,.T.);
#5380=EDGE_CURVE('',#4424,#4422,#2732,.T.);
#5381=EDGE_CURVE('',#4414,#4423,#2733,.T.);
#5382=EDGE_CURVE('',#4416,#4424,#2734,.T.);
#5383=EDGE_CURVE('',#4425,#4425,#3801,.T.);
#5384=EDGE_CURVE('',#4426,#4426,#3802,.T.);
#5385=EDGE_CURVE('',#4426,#4425,#2735,.T.);
#5386=EDGE_CURVE('',#4412,#4426,#2736,.T.);
#5387=EDGE_CURVE('',#4427,#4428,#2737,.T.);
#5388=EDGE_CURVE('',#4428,#4429,#2738,.T.);
#5389=EDGE_CURVE('',#4429,#4430,#2739,.T.);
#5390=EDGE_CURVE('',#4427,#4430,#2740,.T.);
#5391=EDGE_CURVE('',#4428,#4431,#2741,.T.);
#5392=EDGE_CURVE('',#4431,#4432,#2742,.T.);
#5393=EDGE_CURVE('',#4432,#4429,#2743,.T.);
#5394=EDGE_CURVE('',#4431,#4433,#2744,.T.);
#5395=EDGE_CURVE('',#4433,#4434,#2745,.T.);
#5396=EDGE_CURVE('',#4434,#4432,#2746,.T.);
#5397=EDGE_CURVE('',#4433,#4435,#2747,.T.);
#5398=EDGE_CURVE('',#4435,#4436,#2748,.T.);
#5399=EDGE_CURVE('',#4436,#4434,#2749,.T.);
#5400=EDGE_CURVE('',#4435,#4437,#2750,.T.);
#5401=EDGE_CURVE('',#4437,#4438,#2751,.T.);
#5402=EDGE_CURVE('',#4438,#4436,#2752,.T.);
#5403=EDGE_CURVE('',#4437,#4427,#2753,.T.);
#5404=EDGE_CURVE('',#4430,#4438,#2754,.T.);
#5405=EDGE_CURVE('',#4439,#4439,#3803,.T.);
#5406=EDGE_CURVE('',#4440,#4440,#3804,.T.);
#5407=EDGE_CURVE('',#4441,#4441,#3805,.T.);
#5408=EDGE_CURVE('',#4441,#4440,#2755,.T.);
#5409=EDGE_CURVE('',#4442,#4442,#3806,.T.);
#5410=EDGE_CURVE('',#4442,#4441,#2756,.T.);
#5411=EDGE_CURVE('',#4443,#4443,#3807,.T.);
#5412=EDGE_CURVE('',#4443,#4442,#2757,.T.);
#5413=EDGE_CURVE('',#4444,#4444,#3808,.T.);
#5414=EDGE_CURVE('',#4445,#4445,#3809,.F.);
#5415=EDGE_CURVE('',#4445,#4444,#2758,.T.);
#5416=EDGE_CURVE('',#4439,#4445,#2759,.T.);
#5417=EDGE_CURVE('',#4446,#4446,#3810,.T.);
#5418=EDGE_CURVE('',#4447,#4447,#3811,.T.);
#5419=EDGE_CURVE('',#4447,#4446,#2760,.T.);
#5420=EDGE_CURVE('',#4448,#4448,#3812,.T.);
#5421=EDGE_CURVE('',#4448,#4447,#2761,.T.);
#5422=EDGE_CURVE('',#4449,#4449,#3813,.T.);
#5423=EDGE_CURVE('',#4449,#4448,#2762,.T.);
#5424=EDGE_CURVE('',#4450,#4450,#3814,.T.);
#5425=EDGE_CURVE('',#4451,#4451,#3815,.F.);
#5426=EDGE_CURVE('',#4451,#4450,#2763,.T.);
#5427=EDGE_CURVE('',#4452,#4452,#3816,.F.);
#5428=EDGE_CURVE('',#4452,#4451,#2764,.T.);
#5429=EDGE_CURVE('',#4453,#4453,#3817,.T.);
#5430=EDGE_CURVE('',#4453,#4452,#2765,.T.);
#5431=EDGE_CURVE('',#4454,#4455,#2766,.T.);
#5432=EDGE_CURVE('',#4455,#4456,#2767,.T.);
#5433=EDGE_CURVE('',#4456,#4457,#2768,.T.);
#5434=EDGE_CURVE('',#4454,#4457,#2769,.T.);
#5435=EDGE_CURVE('',#4455,#4458,#2770,.T.);
#5436=EDGE_CURVE('',#4458,#4459,#2771,.T.);
#5437=EDGE_CURVE('',#4459,#4456,#2772,.T.);
#5438=EDGE_CURVE('',#4458,#4460,#2773,.T.);
#5439=EDGE_CURVE('',#4460,#4461,#2774,.T.);
#5440=EDGE_CURVE('',#4461,#4459,#2775,.T.);
#5441=EDGE_CURVE('',#4460,#4462,#2776,.T.);
#5442=EDGE_CURVE('',#4462,#4463,#2777,.T.);
#5443=EDGE_CURVE('',#4463,#4461,#2778,.T.);
#5444=EDGE_CURVE('',#4462,#4464,#2779,.T.);
#5445=EDGE_CURVE('',#4464,#4465,#2780,.T.);
#5446=EDGE_CURVE('',#4465,#4463,#2781,.T.);
#5447=EDGE_CURVE('',#4464,#4454,#2782,.T.);
#5448=EDGE_CURVE('',#4457,#4465,#2783,.T.);
#5449=EDGE_CURVE('',#4466,#4466,#3818,.T.);
#5450=EDGE_CURVE('',#4466,#4467,#2784,.T.);
#5451=EDGE_CURVE('',#4467,#4467,#3819,.T.);
#5452=EDGE_CURVE('',#4468,#4468,#3820,.T.);
#5453=EDGE_CURVE('',#4468,#4469,#2785,.T.);
#5454=EDGE_CURVE('',#4469,#4469,#3821,.T.);
#5455=EDGE_CURVE('',#4470,#4471,#2786,.T.);
#5456=EDGE_CURVE('',#4472,#4470,#3822,.T.);
#5457=EDGE_CURVE('',#4473,#4472,#2787,.T.);
#5458=EDGE_CURVE('',#4473,#4471,#3823,.T.);
#5459=EDGE_CURVE('',#4471,#4474,#2788,.T.);
#5460=EDGE_CURVE('',#4475,#4474,#2789,.T.);
#5461=EDGE_CURVE('',#4470,#4475,#2790,.T.);
#5462=EDGE_CURVE('',#4476,#4473,#2791,.T.);
#5463=EDGE_CURVE('',#4474,#4476,#3824,.T.);
#5464=EDGE_CURVE('',#4477,#4472,#2792,.T.);
#5465=EDGE_CURVE('',#4476,#4477,#2793,.T.);
#5466=EDGE_CURVE('',#4475,#4477,#3825,.T.);
#5467=EDGE_CURVE('',#4478,#4478,#3826,.T.);
#5468=EDGE_CURVE('',#4478,#4479,#2794,.T.);
#5469=EDGE_CURVE('',#4479,#4479,#3827,.T.);
#5470=EDGE_CURVE('',#4480,#4480,#3828,.T.);
#5471=EDGE_CURVE('',#4480,#4481,#2795,.T.);
#5472=EDGE_CURVE('',#4481,#4481,#3829,.T.);
#5473=EDGE_CURVE('',#4482,#4482,#3830,.T.);
#5474=EDGE_CURVE('',#4482,#4483,#2796,.T.);
#5475=EDGE_CURVE('',#4483,#4483,#3831,.T.);
#5476=EDGE_CURVE('',#4484,#4484,#3832,.T.);
#5477=EDGE_CURVE('',#4484,#4485,#2797,.T.);
#5478=EDGE_CURVE('',#4485,#4485,#3833,.T.);
#5479=EDGE_CURVE('',#4486,#4486,#3834,.T.);
#5480=EDGE_CURVE('',#4486,#4487,#2798,.T.);
#5481=EDGE_CURVE('',#4487,#4487,#3835,.T.);
#5482=EDGE_CURVE('',#4488,#4489,#2799,.T.);
#5483=EDGE_CURVE('',#4490,#4488,#2800,.T.);
#5484=EDGE_CURVE('',#4491,#4490,#2801,.T.);
#5485=EDGE_CURVE('',#4489,#4491,#2802,.T.);
#5486=EDGE_CURVE('',#4490,#4492,#2803,.T.);
#5487=EDGE_CURVE('',#4493,#4492,#2804,.T.);
#5488=EDGE_CURVE('',#4494,#4493,#2805,.T.);
#5489=EDGE_CURVE('',#4494,#4495,#2806,.T.);
#5490=EDGE_CURVE('',#4491,#4495,#2807,.T.);
#5491=EDGE_CURVE('',#4496,#4488,#2808,.T.);
#5492=EDGE_CURVE('',#4492,#4496,#3836,.T.);
#5493=EDGE_CURVE('',#4497,#4489,#2809,.T.);
#5494=EDGE_CURVE('',#4498,#4497,#2810,.T.);
#5495=EDGE_CURVE('',#4499,#4498,#2811,.T.);
#5496=EDGE_CURVE('',#4496,#4499,#2812,.T.);
#5497=EDGE_CURVE('',#4500,#4501,#2813,.T.);
#5498=EDGE_CURVE('',#4495,#4500,#2814,.T.);
#5499=EDGE_CURVE('',#4501,#4494,#2815,.T.);
#5500=EDGE_CURVE('',#4498,#4502,#2816,.T.);
#5501=EDGE_CURVE('',#4503,#4497,#2817,.T.);
#5502=EDGE_CURVE('',#4502,#4503,#2818,.T.);
#5503=EDGE_CURVE('',#4503,#4500,#3837,.T.);
#5504=EDGE_CURVE('',#4504,#4504,#3838,.T.);
#5505=EDGE_CURVE('',#4504,#4503,#2819,.T.);
#5506=EDGE_CURVE('',#4501,#4502,#3839,.T.);
#5507=EDGE_CURVE('',#4493,#4505,#3840,.T.);
#5508=EDGE_CURVE('',#4505,#4499,#3841,.T.);
#5509=EDGE_CURVE('',#4505,#4506,#2820,.T.);
#5510=EDGE_CURVE('',#4506,#4506,#3842,.T.);
#5511=EDGE_CURVE('',#4507,#4508,#2821,.T.);
#5512=EDGE_CURVE('',#4507,#4508,#3843,.T.);
#5513=EDGE_CURVE('',#4509,#4507,#377,.T.);
#5514=EDGE_CURVE('',#4510,#4509,#3844,.T.);
#5515=EDGE_CURVE('',#4510,#4511,#2822,.T.);
#5516=EDGE_CURVE('',#4511,#4511,#3845,.T.);
#5517=EDGE_CURVE('',#4512,#4510,#3846,.T.);
#5518=EDGE_CURVE('',#4508,#4512,#378,.T.);
#5519=EDGE_CURVE('',#4512,#4509,#2823,.T.);
#5520=EDGE_CURVE('',#4513,#4513,#3847,.T.);
#5521=EDGE_CURVE('',#4513,#4514,#2824,.T.);
#5522=EDGE_CURVE('',#4514,#4514,#3848,.T.);
#5523=EDGE_CURVE('',#4515,#4516,#2825,.T.);
#5524=EDGE_CURVE('',#4516,#4517,#2826,.T.);
#5525=EDGE_CURVE('',#4518,#4517,#2827,.T.);
#5526=EDGE_CURVE('',#4515,#4518,#2828,.T.);
#5527=EDGE_CURVE('',#4519,#4520,#2829,.T.);
#5528=EDGE_CURVE('',#4520,#4515,#2830,.T.);
#5529=EDGE_CURVE('',#4519,#4518,#2831,.T.);
#5530=EDGE_CURVE('',#4521,#4519,#2832,.T.);
#5531=EDGE_CURVE('',#4517,#4521,#2833,.T.);
#5532=EDGE_CURVE('',#4520,#4522,#2834,.T.);
#5533=EDGE_CURVE('',#4516,#4522,#2835,.T.);
#5534=EDGE_CURVE('',#4522,#4521,#2836,.T.);
#5535=EDGE_CURVE('',#4523,#4523,#3849,.T.);
#5536=EDGE_CURVE('',#4524,#4524,#3850,.T.);
#5537=EDGE_CURVE('',#4523,#4525,#2837,.T.);
#5538=EDGE_CURVE('',#4525,#4525,#3851,.T.);
#5539=EDGE_CURVE('',#4526,#4526,#3852,.T.);
#5540=EDGE_CURVE('',#4526,#4524,#2838,.T.);
#5541=EDGE_CURVE('',#4527,#4527,#3853,.T.);
#5542=EDGE_CURVE('',#4527,#4528,#2839,.T.);
#5543=EDGE_CURVE('',#4528,#4528,#3854,.T.);
#5544=EDGE_CURVE('',#4529,#4530,#2840,.T.);
#5545=EDGE_CURVE('',#4529,#4531,#2841,.T.);
#5546=EDGE_CURVE('',#4531,#4532,#2842,.T.);
#5547=EDGE_CURVE('',#4530,#4532,#2843,.T.);
#5548=EDGE_CURVE('',#4533,#4529,#2844,.T.);
#5549=EDGE_CURVE('',#4533,#4534,#2845,.T.);
#5550=EDGE_CURVE('',#4534,#4531,#2846,.T.);
#5551=EDGE_CURVE('',#4535,#4533,#2847,.T.);
#5552=EDGE_CURVE('',#4535,#4536,#2848,.T.);
#5553=EDGE_CURVE('',#4536,#4534,#2849,.T.);
#5554=EDGE_CURVE('',#4537,#4535,#2850,.T.);
#5555=EDGE_CURVE('',#4537,#4538,#2851,.T.);
#5556=EDGE_CURVE('',#4538,#4536,#2852,.T.);
#5557=EDGE_CURVE('',#4539,#4537,#2853,.T.);
#5558=EDGE_CURVE('',#4539,#4540,#2854,.T.);
#5559=EDGE_CURVE('',#4540,#4538,#2855,.T.);
#5560=EDGE_CURVE('',#4530,#4539,#2856,.T.);
#5561=EDGE_CURVE('',#4532,#4540,#2857,.T.);
#5562=EDGE_CURVE('',#4541,#4541,#3855,.T.);
#5563=EDGE_CURVE('',#4542,#4542,#3856,.T.);
#5564=EDGE_CURVE('',#4542,#4541,#2858,.T.);
#5565=EDGE_CURVE('',#4543,#4543,#3857,.F.);
#5566=EDGE_CURVE('',#4543,#4542,#2859,.T.);
#5567=EDGE_CURVE('',#4544,#4544,#3858,.T.);
#5568=EDGE_CURVE('',#4544,#4543,#2860,.T.);
#5569=ORIENTED_EDGE('',*,*,#4545,.F.);
#5570=ORIENTED_EDGE('',*,*,#4546,.T.);
#5571=ORIENTED_EDGE('',*,*,#4547,.F.);
#5572=ORIENTED_EDGE('',*,*,#4546,.F.);
#5573=ORIENTED_EDGE('',*,*,#4548,.F.);
#5574=ORIENTED_EDGE('',*,*,#4549,.T.);
#5575=ORIENTED_EDGE('',*,*,#4550,.F.);
#5576=ORIENTED_EDGE('',*,*,#4549,.F.);
#5577=ORIENTED_EDGE('',*,*,#4551,.F.);
#5578=ORIENTED_EDGE('',*,*,#4552,.T.);
#5579=ORIENTED_EDGE('',*,*,#4553,.F.);
#5580=ORIENTED_EDGE('',*,*,#4552,.F.);
#5581=ORIENTED_EDGE('',*,*,#4554,.F.);
#5582=ORIENTED_EDGE('',*,*,#4555,.T.);
#5583=ORIENTED_EDGE('',*,*,#4556,.F.);
#5584=ORIENTED_EDGE('',*,*,#4555,.F.);
#5585=ORIENTED_EDGE('',*,*,#4557,.F.);
#5586=ORIENTED_EDGE('',*,*,#4558,.T.);
#5587=ORIENTED_EDGE('',*,*,#4559,.F.);
#5588=ORIENTED_EDGE('',*,*,#4558,.F.);
#5589=ORIENTED_EDGE('',*,*,#4560,.F.);
#5590=ORIENTED_EDGE('',*,*,#4561,.T.);
#5591=ORIENTED_EDGE('',*,*,#4562,.F.);
#5592=ORIENTED_EDGE('',*,*,#4561,.F.);
#5593=ORIENTED_EDGE('',*,*,#4563,.F.);
#5594=ORIENTED_EDGE('',*,*,#4564,.T.);
#5595=ORIENTED_EDGE('',*,*,#4565,.F.);
#5596=ORIENTED_EDGE('',*,*,#4564,.F.);
#5597=ORIENTED_EDGE('',*,*,#4566,.F.);
#5598=ORIENTED_EDGE('',*,*,#4567,.T.);
#5599=ORIENTED_EDGE('',*,*,#4568,.F.);
#5600=ORIENTED_EDGE('',*,*,#4567,.F.);
#5601=ORIENTED_EDGE('',*,*,#4569,.F.);
#5602=ORIENTED_EDGE('',*,*,#4570,.T.);
#5603=ORIENTED_EDGE('',*,*,#4571,.F.);
#5604=ORIENTED_EDGE('',*,*,#4570,.F.);
#5605=ORIENTED_EDGE('',*,*,#4572,.F.);
#5606=ORIENTED_EDGE('',*,*,#4573,.T.);
#5607=ORIENTED_EDGE('',*,*,#4574,.F.);
#5608=ORIENTED_EDGE('',*,*,#4573,.F.);
#5609=ORIENTED_EDGE('',*,*,#4575,.F.);
#5610=ORIENTED_EDGE('',*,*,#4576,.T.);
#5611=ORIENTED_EDGE('',*,*,#4577,.F.);
#5612=ORIENTED_EDGE('',*,*,#4576,.F.);
#5613=ORIENTED_EDGE('',*,*,#4578,.F.);
#5614=ORIENTED_EDGE('',*,*,#4579,.T.);
#5615=ORIENTED_EDGE('',*,*,#4580,.F.);
#5616=ORIENTED_EDGE('',*,*,#4579,.F.);
#5617=ORIENTED_EDGE('',*,*,#4581,.T.);
#5618=ORIENTED_EDGE('',*,*,#4582,.T.);
#5619=ORIENTED_EDGE('',*,*,#4583,.F.);
#5620=ORIENTED_EDGE('',*,*,#4584,.F.);
#5621=ORIENTED_EDGE('',*,*,#4585,.T.);
#5622=ORIENTED_EDGE('',*,*,#4584,.T.);
#5623=ORIENTED_EDGE('',*,*,#4586,.F.);
#5624=ORIENTED_EDGE('',*,*,#4587,.F.);
#5625=ORIENTED_EDGE('',*,*,#4588,.T.);
#5626=ORIENTED_EDGE('',*,*,#4587,.T.);
#5627=ORIENTED_EDGE('',*,*,#4589,.F.);
#5628=ORIENTED_EDGE('',*,*,#4590,.F.);
#5629=ORIENTED_EDGE('',*,*,#4591,.T.);
#5630=ORIENTED_EDGE('',*,*,#4590,.T.);
#5631=ORIENTED_EDGE('',*,*,#4592,.F.);
#5632=ORIENTED_EDGE('',*,*,#4582,.F.);
#5633=ORIENTED_EDGE('',*,*,#4592,.T.);
#5634=ORIENTED_EDGE('',*,*,#4589,.T.);
#5635=ORIENTED_EDGE('',*,*,#4586,.T.);
#5636=ORIENTED_EDGE('',*,*,#4583,.T.);
#5637=ORIENTED_EDGE('',*,*,#4553,.T.);
#5638=ORIENTED_EDGE('',*,*,#4556,.T.);
#5639=ORIENTED_EDGE('',*,*,#4580,.T.);
#5640=ORIENTED_EDGE('',*,*,#4577,.T.);
#5641=ORIENTED_EDGE('',*,*,#4574,.T.);
#5642=ORIENTED_EDGE('',*,*,#4571,.T.);
#5643=ORIENTED_EDGE('',*,*,#4568,.T.);
#5644=ORIENTED_EDGE('',*,*,#4565,.T.);
#5645=ORIENTED_EDGE('',*,*,#4562,.T.);
#5646=ORIENTED_EDGE('',*,*,#4559,.T.);
#5647=ORIENTED_EDGE('',*,*,#4550,.T.);
#5648=ORIENTED_EDGE('',*,*,#4547,.T.);
#5649=ORIENTED_EDGE('',*,*,#4591,.F.);
#5650=ORIENTED_EDGE('',*,*,#4581,.F.);
#5651=ORIENTED_EDGE('',*,*,#4585,.F.);
#5652=ORIENTED_EDGE('',*,*,#4588,.F.);
#5653=ORIENTED_EDGE('',*,*,#4551,.T.);
#5654=ORIENTED_EDGE('',*,*,#4554,.T.);
#5655=ORIENTED_EDGE('',*,*,#4578,.T.);
#5656=ORIENTED_EDGE('',*,*,#4575,.T.);
#5657=ORIENTED_EDGE('',*,*,#4572,.T.);
#5658=ORIENTED_EDGE('',*,*,#4569,.T.);
#5659=ORIENTED_EDGE('',*,*,#4566,.T.);
#5660=ORIENTED_EDGE('',*,*,#4563,.T.);
#5661=ORIENTED_EDGE('',*,*,#4560,.T.);
#5662=ORIENTED_EDGE('',*,*,#4557,.T.);
#5663=ORIENTED_EDGE('',*,*,#4548,.T.);
#5664=ORIENTED_EDGE('',*,*,#4545,.T.);
#5665=ORIENTED_EDGE('',*,*,#4593,.F.);
#5666=ORIENTED_EDGE('',*,*,#4594,.T.);
#5667=ORIENTED_EDGE('',*,*,#4595,.F.);
#5668=ORIENTED_EDGE('',*,*,#4594,.F.);
#5669=ORIENTED_EDGE('',*,*,#4596,.F.);
#5670=ORIENTED_EDGE('',*,*,#4597,.T.);
#5671=ORIENTED_EDGE('',*,*,#4598,.F.);
#5672=ORIENTED_EDGE('',*,*,#4597,.F.);
#5673=ORIENTED_EDGE('',*,*,#4599,.F.);
#5674=ORIENTED_EDGE('',*,*,#4600,.T.);
#5675=ORIENTED_EDGE('',*,*,#4601,.F.);
#5676=ORIENTED_EDGE('',*,*,#4600,.F.);
#5677=ORIENTED_EDGE('',*,*,#4602,.F.);
#5678=ORIENTED_EDGE('',*,*,#4603,.T.);
#5679=ORIENTED_EDGE('',*,*,#4604,.F.);
#5680=ORIENTED_EDGE('',*,*,#4603,.F.);
#5681=ORIENTED_EDGE('',*,*,#4605,.T.);
#5682=ORIENTED_EDGE('',*,*,#4606,.T.);
#5683=ORIENTED_EDGE('',*,*,#4607,.F.);
#5684=ORIENTED_EDGE('',*,*,#4608,.F.);
#5685=ORIENTED_EDGE('',*,*,#4609,.T.);
#5686=ORIENTED_EDGE('',*,*,#4608,.T.);
#5687=ORIENTED_EDGE('',*,*,#4610,.F.);
#5688=ORIENTED_EDGE('',*,*,#4611,.F.);
#5689=ORIENTED_EDGE('',*,*,#4612,.T.);
#5690=ORIENTED_EDGE('',*,*,#4611,.T.);
#5691=ORIENTED_EDGE('',*,*,#4613,.F.);
#5692=ORIENTED_EDGE('',*,*,#4614,.F.);
#5693=ORIENTED_EDGE('',*,*,#4615,.T.);
#5694=ORIENTED_EDGE('',*,*,#4614,.T.);
#5695=ORIENTED_EDGE('',*,*,#4616,.F.);
#5696=ORIENTED_EDGE('',*,*,#4606,.F.);
#5697=ORIENTED_EDGE('',*,*,#4616,.T.);
#5698=ORIENTED_EDGE('',*,*,#4613,.T.);
#5699=ORIENTED_EDGE('',*,*,#4610,.T.);
#5700=ORIENTED_EDGE('',*,*,#4607,.T.);
#5701=ORIENTED_EDGE('',*,*,#4595,.T.);
#5702=ORIENTED_EDGE('',*,*,#4598,.T.);
#5703=ORIENTED_EDGE('',*,*,#4601,.T.);
#5704=ORIENTED_EDGE('',*,*,#4604,.T.);
#5705=ORIENTED_EDGE('',*,*,#4615,.F.);
#5706=ORIENTED_EDGE('',*,*,#4605,.F.);
#5707=ORIENTED_EDGE('',*,*,#4609,.F.);
#5708=ORIENTED_EDGE('',*,*,#4612,.F.);
#5709=ORIENTED_EDGE('',*,*,#4593,.T.);
#5710=ORIENTED_EDGE('',*,*,#4596,.T.);
#5711=ORIENTED_EDGE('',*,*,#4599,.T.);
#5712=ORIENTED_EDGE('',*,*,#4602,.T.);
#5713=ORIENTED_EDGE('',*,*,#4617,.T.);
#5714=ORIENTED_EDGE('',*,*,#4618,.T.);
#5715=ORIENTED_EDGE('',*,*,#4619,.F.);
#5716=ORIENTED_EDGE('',*,*,#4620,.F.);
#5717=ORIENTED_EDGE('',*,*,#4621,.T.);
#5718=ORIENTED_EDGE('',*,*,#4620,.T.);
#5719=ORIENTED_EDGE('',*,*,#4622,.F.);
#5720=ORIENTED_EDGE('',*,*,#4623,.F.);
#5721=ORIENTED_EDGE('',*,*,#4624,.T.);
#5722=ORIENTED_EDGE('',*,*,#4623,.T.);
#5723=ORIENTED_EDGE('',*,*,#4625,.F.);
#5724=ORIENTED_EDGE('',*,*,#4626,.F.);
#5725=ORIENTED_EDGE('',*,*,#4627,.T.);
#5726=ORIENTED_EDGE('',*,*,#4626,.T.);
#5727=ORIENTED_EDGE('',*,*,#4628,.F.);
#5728=ORIENTED_EDGE('',*,*,#4618,.F.);
#5729=ORIENTED_EDGE('',*,*,#4628,.T.);
#5730=ORIENTED_EDGE('',*,*,#4625,.T.);
#5731=ORIENTED_EDGE('',*,*,#4622,.T.);
#5732=ORIENTED_EDGE('',*,*,#4619,.T.);
#5733=ORIENTED_EDGE('',*,*,#4627,.F.);
#5734=ORIENTED_EDGE('',*,*,#4617,.F.);
#5735=ORIENTED_EDGE('',*,*,#4621,.F.);
#5736=ORIENTED_EDGE('',*,*,#4624,.F.);
#5737=ORIENTED_EDGE('',*,*,#4629,.T.);
#5738=ORIENTED_EDGE('',*,*,#4630,.T.);
#5739=ORIENTED_EDGE('',*,*,#4631,.F.);
#5740=ORIENTED_EDGE('',*,*,#4632,.F.);
#5741=ORIENTED_EDGE('',*,*,#4633,.T.);
#5742=ORIENTED_EDGE('',*,*,#4632,.T.);
#5743=ORIENTED_EDGE('',*,*,#4634,.F.);
#5744=ORIENTED_EDGE('',*,*,#4635,.F.);
#5745=ORIENTED_EDGE('',*,*,#4636,.T.);
#5746=ORIENTED_EDGE('',*,*,#4635,.T.);
#5747=ORIENTED_EDGE('',*,*,#4637,.F.);
#5748=ORIENTED_EDGE('',*,*,#4638,.F.);
#5749=ORIENTED_EDGE('',*,*,#4639,.T.);
#5750=ORIENTED_EDGE('',*,*,#4638,.T.);
#5751=ORIENTED_EDGE('',*,*,#4640,.F.);
#5752=ORIENTED_EDGE('',*,*,#4630,.F.);
#5753=ORIENTED_EDGE('',*,*,#4640,.T.);
#5754=ORIENTED_EDGE('',*,*,#4637,.T.);
#5755=ORIENTED_EDGE('',*,*,#4634,.T.);
#5756=ORIENTED_EDGE('',*,*,#4631,.T.);
#5757=ORIENTED_EDGE('',*,*,#4639,.F.);
#5758=ORIENTED_EDGE('',*,*,#4629,.F.);
#5759=ORIENTED_EDGE('',*,*,#4633,.F.);
#5760=ORIENTED_EDGE('',*,*,#4636,.F.);
#5761=ORIENTED_EDGE('',*,*,#4641,.F.);
#5762=ORIENTED_EDGE('',*,*,#4642,.T.);
#5763=ORIENTED_EDGE('',*,*,#4643,.F.);
#5764=ORIENTED_EDGE('',*,*,#4642,.F.);
#5765=ORIENTED_EDGE('',*,*,#4644,.F.);
#5766=ORIENTED_EDGE('',*,*,#4645,.T.);
#5767=ORIENTED_EDGE('',*,*,#4646,.F.);
#5768=ORIENTED_EDGE('',*,*,#4645,.F.);
#5769=ORIENTED_EDGE('',*,*,#4644,.T.);
#5770=ORIENTED_EDGE('',*,*,#4647,.F.);
#5771=ORIENTED_EDGE('',*,*,#4648,.T.);
#5772=ORIENTED_EDGE('',*,*,#4649,.F.);
#5773=ORIENTED_EDGE('',*,*,#4648,.F.);
#5774=ORIENTED_EDGE('',*,*,#4647,.T.);
#5775=ORIENTED_EDGE('',*,*,#4650,.F.);
#5776=ORIENTED_EDGE('',*,*,#4651,.T.);
#5777=ORIENTED_EDGE('',*,*,#4652,.F.);
#5778=ORIENTED_EDGE('',*,*,#4651,.F.);
#5779=ORIENTED_EDGE('',*,*,#4650,.T.);
#5780=ORIENTED_EDGE('',*,*,#4653,.F.);
#5781=ORIENTED_EDGE('',*,*,#4654,.T.);
#5782=ORIENTED_EDGE('',*,*,#4655,.F.);
#5783=ORIENTED_EDGE('',*,*,#4654,.F.);
#5784=ORIENTED_EDGE('',*,*,#4653,.T.);
#5785=ORIENTED_EDGE('',*,*,#4656,.F.);
#5786=ORIENTED_EDGE('',*,*,#4657,.T.);
#5787=ORIENTED_EDGE('',*,*,#4658,.F.);
#5788=ORIENTED_EDGE('',*,*,#4657,.F.);
#5789=ORIENTED_EDGE('',*,*,#4659,.F.);
#5790=ORIENTED_EDGE('',*,*,#4660,.T.);
#5791=ORIENTED_EDGE('',*,*,#4661,.F.);
#5792=ORIENTED_EDGE('',*,*,#4660,.F.);
#5793=ORIENTED_EDGE('',*,*,#4662,.F.);
#5794=ORIENTED_EDGE('',*,*,#4663,.T.);
#5795=ORIENTED_EDGE('',*,*,#4664,.F.);
#5796=ORIENTED_EDGE('',*,*,#4663,.F.);
#5797=ORIENTED_EDGE('',*,*,#4665,.F.);
#5798=ORIENTED_EDGE('',*,*,#4666,.T.);
#5799=ORIENTED_EDGE('',*,*,#4667,.F.);
#5800=ORIENTED_EDGE('',*,*,#4666,.F.);
#5801=ORIENTED_EDGE('',*,*,#4668,.F.);
#5802=ORIENTED_EDGE('',*,*,#4669,.T.);
#5803=ORIENTED_EDGE('',*,*,#4670,.F.);
#5804=ORIENTED_EDGE('',*,*,#4669,.F.);
#5805=ORIENTED_EDGE('',*,*,#4671,.F.);
#5806=ORIENTED_EDGE('',*,*,#4672,.T.);
#5807=ORIENTED_EDGE('',*,*,#4673,.F.);
#5808=ORIENTED_EDGE('',*,*,#4672,.F.);
#5809=ORIENTED_EDGE('',*,*,#4674,.F.);
#5810=ORIENTED_EDGE('',*,*,#4675,.T.);
#5811=ORIENTED_EDGE('',*,*,#4676,.F.);
#5812=ORIENTED_EDGE('',*,*,#4675,.F.);
#5813=ORIENTED_EDGE('',*,*,#4677,.F.);
#5814=ORIENTED_EDGE('',*,*,#4678,.T.);
#5815=ORIENTED_EDGE('',*,*,#4679,.F.);
#5816=ORIENTED_EDGE('',*,*,#4678,.F.);
#5817=ORIENTED_EDGE('',*,*,#4680,.F.);
#5818=ORIENTED_EDGE('',*,*,#4681,.T.);
#5819=ORIENTED_EDGE('',*,*,#4682,.F.);
#5820=ORIENTED_EDGE('',*,*,#4681,.F.);
#5821=ORIENTED_EDGE('',*,*,#4680,.T.);
#5822=ORIENTED_EDGE('',*,*,#4683,.F.);
#5823=ORIENTED_EDGE('',*,*,#4684,.F.);
#5824=ORIENTED_EDGE('',*,*,#4685,.T.);
#5825=ORIENTED_EDGE('',*,*,#4683,.T.);
#5826=ORIENTED_EDGE('',*,*,#4685,.F.);
#5827=ORIENTED_EDGE('',*,*,#4686,.F.);
#5828=ORIENTED_EDGE('',*,*,#4687,.T.);
#5829=ORIENTED_EDGE('',*,*,#4688,.F.);
#5830=ORIENTED_EDGE('',*,*,#4687,.F.);
#5831=ORIENTED_EDGE('',*,*,#4689,.F.);
#5832=ORIENTED_EDGE('',*,*,#4690,.T.);
#5833=ORIENTED_EDGE('',*,*,#4691,.F.);
#5834=ORIENTED_EDGE('',*,*,#4692,.F.);
#5835=ORIENTED_EDGE('',*,*,#4689,.T.);
#5836=ORIENTED_EDGE('',*,*,#4693,.T.);
#5837=ORIENTED_EDGE('',*,*,#4694,.T.);
#5838=ORIENTED_EDGE('',*,*,#4695,.F.);
#5839=ORIENTED_EDGE('',*,*,#4696,.F.);
#5840=ORIENTED_EDGE('',*,*,#4697,.T.);
#5841=ORIENTED_EDGE('',*,*,#4698,.T.);
#5842=ORIENTED_EDGE('',*,*,#4699,.T.);
#5843=ORIENTED_EDGE('',*,*,#4700,.F.);
#5844=ORIENTED_EDGE('',*,*,#4701,.T.);
#5845=ORIENTED_EDGE('',*,*,#4641,.T.);
#5846=ORIENTED_EDGE('',*,*,#4686,.T.);
#5847=ORIENTED_EDGE('',*,*,#4665,.T.);
#5848=ORIENTED_EDGE('',*,*,#4662,.T.);
#5849=ORIENTED_EDGE('',*,*,#4659,.T.);
#5850=ORIENTED_EDGE('',*,*,#4656,.T.);
#5851=ORIENTED_EDGE('',*,*,#4692,.T.);
#5852=ORIENTED_EDGE('',*,*,#4702,.F.);
#5853=ORIENTED_EDGE('',*,*,#4703,.F.);
#5854=ORIENTED_EDGE('',*,*,#4693,.F.);
#5855=ORIENTED_EDGE('',*,*,#4682,.T.);
#5856=ORIENTED_EDGE('',*,*,#4655,.T.);
#5857=ORIENTED_EDGE('',*,*,#4652,.T.);
#5858=ORIENTED_EDGE('',*,*,#4649,.T.);
#5859=ORIENTED_EDGE('',*,*,#4646,.T.);
#5860=ORIENTED_EDGE('',*,*,#4704,.T.);
#5861=ORIENTED_EDGE('',*,*,#4705,.T.);
#5862=ORIENTED_EDGE('',*,*,#4706,.T.);
#5863=ORIENTED_EDGE('',*,*,#4707,.T.);
#5864=ORIENTED_EDGE('',*,*,#4708,.F.);
#5865=ORIENTED_EDGE('',*,*,#4709,.F.);
#5866=ORIENTED_EDGE('',*,*,#4697,.F.);
#5867=ORIENTED_EDGE('',*,*,#4710,.F.);
#5868=ORIENTED_EDGE('',*,*,#4679,.T.);
#5869=ORIENTED_EDGE('',*,*,#4676,.T.);
#5870=ORIENTED_EDGE('',*,*,#4673,.T.);
#5871=ORIENTED_EDGE('',*,*,#4670,.T.);
#5872=ORIENTED_EDGE('',*,*,#4711,.T.);
#5873=ORIENTED_EDGE('',*,*,#4712,.T.);
#5874=ORIENTED_EDGE('',*,*,#4707,.F.);
#5875=ORIENTED_EDGE('',*,*,#4713,.F.);
#5876=ORIENTED_EDGE('',*,*,#4714,.T.);
#5877=ORIENTED_EDGE('',*,*,#4713,.T.);
#5878=ORIENTED_EDGE('',*,*,#4706,.F.);
#5879=ORIENTED_EDGE('',*,*,#4715,.F.);
#5880=ORIENTED_EDGE('',*,*,#4716,.T.);
#5881=ORIENTED_EDGE('',*,*,#4715,.T.);
#5882=ORIENTED_EDGE('',*,*,#4705,.F.);
#5883=ORIENTED_EDGE('',*,*,#4717,.F.);
#5884=ORIENTED_EDGE('',*,*,#4718,.T.);
#5885=ORIENTED_EDGE('',*,*,#4717,.T.);
#5886=ORIENTED_EDGE('',*,*,#4704,.F.);
#5887=ORIENTED_EDGE('',*,*,#4712,.F.);
#5888=ORIENTED_EDGE('',*,*,#4709,.T.);
#5889=ORIENTED_EDGE('',*,*,#4719,.T.);
#5890=ORIENTED_EDGE('',*,*,#4720,.T.);
#5891=ORIENTED_EDGE('',*,*,#4698,.F.);
#5892=ORIENTED_EDGE('',*,*,#4721,.F.);
#5893=ORIENTED_EDGE('',*,*,#4700,.T.);
#5894=ORIENTED_EDGE('',*,*,#4722,.F.);
#5895=ORIENTED_EDGE('',*,*,#4723,.F.);
#5896=ORIENTED_EDGE('',*,*,#4691,.T.);
#5897=ORIENTED_EDGE('',*,*,#4724,.T.);
#5898=ORIENTED_EDGE('',*,*,#4723,.T.);
#5899=ORIENTED_EDGE('',*,*,#4725,.T.);
#5900=ORIENTED_EDGE('',*,*,#4719,.F.);
#5901=ORIENTED_EDGE('',*,*,#4708,.T.);
#5902=ORIENTED_EDGE('',*,*,#4726,.T.);
#5903=ORIENTED_EDGE('',*,*,#4727,.F.);
#5904=ORIENTED_EDGE('',*,*,#4728,.F.);
#5905=ORIENTED_EDGE('',*,*,#4702,.T.);
#5906=ORIENTED_EDGE('',*,*,#4643,.T.);
#5907=ORIENTED_EDGE('',*,*,#4688,.T.);
#5908=ORIENTED_EDGE('',*,*,#4667,.T.);
#5909=ORIENTED_EDGE('',*,*,#4664,.T.);
#5910=ORIENTED_EDGE('',*,*,#4661,.T.);
#5911=ORIENTED_EDGE('',*,*,#4658,.T.);
#5912=ORIENTED_EDGE('',*,*,#4722,.T.);
#5913=ORIENTED_EDGE('',*,*,#4699,.F.);
#5914=ORIENTED_EDGE('',*,*,#4720,.F.);
#5915=ORIENTED_EDGE('',*,*,#4725,.F.);
#5916=ORIENTED_EDGE('',*,*,#4701,.F.);
#5917=ORIENTED_EDGE('',*,*,#4721,.T.);
#5918=ORIENTED_EDGE('',*,*,#4724,.F.);
#5919=ORIENTED_EDGE('',*,*,#4690,.F.);
#5920=ORIENTED_EDGE('',*,*,#4684,.T.);
#5921=ORIENTED_EDGE('',*,*,#4703,.T.);
#5922=ORIENTED_EDGE('',*,*,#4728,.T.);
#5923=ORIENTED_EDGE('',*,*,#4729,.F.);
#5924=ORIENTED_EDGE('',*,*,#4694,.F.);
#5925=ORIENTED_EDGE('',*,*,#4710,.T.);
#5926=ORIENTED_EDGE('',*,*,#4696,.T.);
#5927=ORIENTED_EDGE('',*,*,#4730,.F.);
#5928=ORIENTED_EDGE('',*,*,#4726,.F.);
#5929=ORIENTED_EDGE('',*,*,#4730,.T.);
#5930=ORIENTED_EDGE('',*,*,#4695,.T.);
#5931=ORIENTED_EDGE('',*,*,#4729,.T.);
#5932=ORIENTED_EDGE('',*,*,#4727,.T.);
#5933=ORIENTED_EDGE('',*,*,#4718,.F.);
#5934=ORIENTED_EDGE('',*,*,#4711,.F.);
#5935=ORIENTED_EDGE('',*,*,#4714,.F.);
#5936=ORIENTED_EDGE('',*,*,#4716,.F.);
#5937=ORIENTED_EDGE('',*,*,#4668,.T.);
#5938=ORIENTED_EDGE('',*,*,#4671,.T.);
#5939=ORIENTED_EDGE('',*,*,#4674,.T.);
#5940=ORIENTED_EDGE('',*,*,#4677,.T.);
#5941=ORIENTED_EDGE('',*,*,#4731,.F.);
#5942=ORIENTED_EDGE('',*,*,#4732,.T.);
#5943=ORIENTED_EDGE('',*,*,#4733,.F.);
#5944=ORIENTED_EDGE('',*,*,#4732,.F.);
#5945=ORIENTED_EDGE('',*,*,#4734,.F.);
#5946=ORIENTED_EDGE('',*,*,#4735,.T.);
#5947=ORIENTED_EDGE('',*,*,#4736,.F.);
#5948=ORIENTED_EDGE('',*,*,#4735,.F.);
#5949=ORIENTED_EDGE('',*,*,#4737,.F.);
#5950=ORIENTED_EDGE('',*,*,#4738,.T.);
#5951=ORIENTED_EDGE('',*,*,#4739,.F.);
#5952=ORIENTED_EDGE('',*,*,#4738,.F.);
#5953=ORIENTED_EDGE('',*,*,#4740,.F.);
#5954=ORIENTED_EDGE('',*,*,#4741,.T.);
#5955=ORIENTED_EDGE('',*,*,#4742,.F.);
#5956=ORIENTED_EDGE('',*,*,#4741,.F.);
#5957=ORIENTED_EDGE('',*,*,#4743,.F.);
#5958=ORIENTED_EDGE('',*,*,#4744,.T.);
#5959=ORIENTED_EDGE('',*,*,#4745,.F.);
#5960=ORIENTED_EDGE('',*,*,#4744,.F.);
#5961=ORIENTED_EDGE('',*,*,#4743,.T.);
#5962=ORIENTED_EDGE('',*,*,#4746,.T.);
#5963=ORIENTED_EDGE('',*,*,#4746,.F.);
#5964=ORIENTED_EDGE('',*,*,#4747,.T.);
#5965=ORIENTED_EDGE('',*,*,#4748,.T.);
#5966=ORIENTED_EDGE('',*,*,#4747,.F.);
#5967=ORIENTED_EDGE('',*,*,#4749,.F.);
#5968=ORIENTED_EDGE('',*,*,#4750,.T.);
#5969=ORIENTED_EDGE('',*,*,#4751,.T.);
#5970=ORIENTED_EDGE('',*,*,#4750,.F.);
#5971=ORIENTED_EDGE('',*,*,#4749,.T.);
#5972=ORIENTED_EDGE('',*,*,#4745,.T.);
#5973=ORIENTED_EDGE('',*,*,#4742,.T.);
#5974=ORIENTED_EDGE('',*,*,#4739,.T.);
#5975=ORIENTED_EDGE('',*,*,#4736,.T.);
#5976=ORIENTED_EDGE('',*,*,#4733,.T.);
#5977=ORIENTED_EDGE('',*,*,#4751,.F.);
#5978=ORIENTED_EDGE('',*,*,#4748,.F.);
#5979=ORIENTED_EDGE('',*,*,#4740,.T.);
#5980=ORIENTED_EDGE('',*,*,#4737,.T.);
#5981=ORIENTED_EDGE('',*,*,#4734,.T.);
#5982=ORIENTED_EDGE('',*,*,#4731,.T.);
#5983=ORIENTED_EDGE('',*,*,#4752,.F.);
#5984=ORIENTED_EDGE('',*,*,#4753,.T.);
#5985=ORIENTED_EDGE('',*,*,#4754,.F.);
#5986=ORIENTED_EDGE('',*,*,#4753,.F.);
#5987=ORIENTED_EDGE('',*,*,#4755,.F.);
#5988=ORIENTED_EDGE('',*,*,#4756,.T.);
#5989=ORIENTED_EDGE('',*,*,#4757,.F.);
#5990=ORIENTED_EDGE('',*,*,#4756,.F.);
#5991=ORIENTED_EDGE('',*,*,#4758,.F.);
#5992=ORIENTED_EDGE('',*,*,#4759,.T.);
#5993=ORIENTED_EDGE('',*,*,#4760,.F.);
#5994=ORIENTED_EDGE('',*,*,#4759,.F.);
#5995=ORIENTED_EDGE('',*,*,#4761,.F.);
#5996=ORIENTED_EDGE('',*,*,#4762,.T.);
#5997=ORIENTED_EDGE('',*,*,#4763,.F.);
#5998=ORIENTED_EDGE('',*,*,#4762,.F.);
#5999=ORIENTED_EDGE('',*,*,#4764,.F.);
#6000=ORIENTED_EDGE('',*,*,#4765,.T.);
#6001=ORIENTED_EDGE('',*,*,#4766,.T.);
#6002=ORIENTED_EDGE('',*,*,#4765,.F.);
#6003=ORIENTED_EDGE('',*,*,#4766,.F.);
#6004=ORIENTED_EDGE('',*,*,#4767,.F.);
#6005=ORIENTED_EDGE('',*,*,#4768,.F.);
#6006=ORIENTED_EDGE('',*,*,#4769,.T.);
#6007=ORIENTED_EDGE('',*,*,#4767,.T.);
#6008=ORIENTED_EDGE('',*,*,#4769,.F.);
#6009=ORIENTED_EDGE('',*,*,#4770,.F.);
#6010=ORIENTED_EDGE('',*,*,#4771,.T.);
#6011=ORIENTED_EDGE('',*,*,#4772,.T.);
#6012=ORIENTED_EDGE('',*,*,#4771,.F.);
#6013=ORIENTED_EDGE('',*,*,#4770,.T.);
#6014=ORIENTED_EDGE('',*,*,#4768,.T.);
#6015=ORIENTED_EDGE('',*,*,#4763,.T.);
#6016=ORIENTED_EDGE('',*,*,#4760,.T.);
#6017=ORIENTED_EDGE('',*,*,#4757,.T.);
#6018=ORIENTED_EDGE('',*,*,#4754,.T.);
#6019=ORIENTED_EDGE('',*,*,#4772,.F.);
#6020=ORIENTED_EDGE('',*,*,#4764,.T.);
#6021=ORIENTED_EDGE('',*,*,#4761,.T.);
#6022=ORIENTED_EDGE('',*,*,#4758,.T.);
#6023=ORIENTED_EDGE('',*,*,#4755,.T.);
#6024=ORIENTED_EDGE('',*,*,#4752,.T.);
#6025=ORIENTED_EDGE('',*,*,#4773,.F.);
#6026=ORIENTED_EDGE('',*,*,#4774,.T.);
#6027=ORIENTED_EDGE('',*,*,#4775,.F.);
#6028=ORIENTED_EDGE('',*,*,#4774,.F.);
#6029=ORIENTED_EDGE('',*,*,#4773,.T.);
#6030=ORIENTED_EDGE('',*,*,#4776,.F.);
#6031=ORIENTED_EDGE('',*,*,#4777,.F.);
#6032=ORIENTED_EDGE('',*,*,#4778,.T.);
#6033=ORIENTED_EDGE('',*,*,#4779,.F.);
#6034=ORIENTED_EDGE('',*,*,#4778,.F.);
#6035=ORIENTED_EDGE('',*,*,#4777,.T.);
#6036=ORIENTED_EDGE('',*,*,#4780,.F.);
#6037=ORIENTED_EDGE('',*,*,#4781,.F.);
#6038=ORIENTED_EDGE('',*,*,#4782,.T.);
#6039=ORIENTED_EDGE('',*,*,#4783,.F.);
#6040=ORIENTED_EDGE('',*,*,#4782,.F.);
#6041=ORIENTED_EDGE('',*,*,#4781,.T.);
#6042=ORIENTED_EDGE('',*,*,#4784,.F.);
#6043=ORIENTED_EDGE('',*,*,#4785,.F.);
#6044=ORIENTED_EDGE('',*,*,#4786,.T.);
#6045=ORIENTED_EDGE('',*,*,#4787,.F.);
#6046=ORIENTED_EDGE('',*,*,#4786,.F.);
#6047=ORIENTED_EDGE('',*,*,#4785,.T.);
#6048=ORIENTED_EDGE('',*,*,#4788,.F.);
#6049=ORIENTED_EDGE('',*,*,#4789,.F.);
#6050=ORIENTED_EDGE('',*,*,#4790,.T.);
#6051=ORIENTED_EDGE('',*,*,#4776,.T.);
#6052=ORIENTED_EDGE('',*,*,#4790,.F.);
#6053=ORIENTED_EDGE('',*,*,#4791,.F.);
#6054=ORIENTED_EDGE('',*,*,#4792,.T.);
#6055=ORIENTED_EDGE('',*,*,#4780,.T.);
#6056=ORIENTED_EDGE('',*,*,#4792,.F.);
#6057=ORIENTED_EDGE('',*,*,#4793,.F.);
#6058=ORIENTED_EDGE('',*,*,#4794,.T.);
#6059=ORIENTED_EDGE('',*,*,#4784,.T.);
#6060=ORIENTED_EDGE('',*,*,#4794,.F.);
#6061=ORIENTED_EDGE('',*,*,#4795,.F.);
#6062=ORIENTED_EDGE('',*,*,#4796,.T.);
#6063=ORIENTED_EDGE('',*,*,#4788,.T.);
#6064=ORIENTED_EDGE('',*,*,#4796,.F.);
#6065=ORIENTED_EDGE('',*,*,#4797,.F.);
#6066=ORIENTED_EDGE('',*,*,#4798,.T.);
#6067=ORIENTED_EDGE('',*,*,#4799,.T.);
#6068=ORIENTED_EDGE('',*,*,#4798,.F.);
#6069=ORIENTED_EDGE('',*,*,#4799,.F.);
#6070=ORIENTED_EDGE('',*,*,#4800,.F.);
#6071=ORIENTED_EDGE('',*,*,#4801,.F.);
#6072=ORIENTED_EDGE('',*,*,#4802,.T.);
#6073=ORIENTED_EDGE('',*,*,#4800,.T.);
#6074=ORIENTED_EDGE('',*,*,#4802,.F.);
#6075=ORIENTED_EDGE('',*,*,#4803,.F.);
#6076=ORIENTED_EDGE('',*,*,#4804,.T.);
#6077=ORIENTED_EDGE('',*,*,#4805,.T.);
#6078=ORIENTED_EDGE('',*,*,#4804,.F.);
#6079=ORIENTED_EDGE('',*,*,#4803,.T.);
#6080=ORIENTED_EDGE('',*,*,#4801,.T.);
#6081=ORIENTED_EDGE('',*,*,#4787,.T.);
#6082=ORIENTED_EDGE('',*,*,#4783,.T.);
#6083=ORIENTED_EDGE('',*,*,#4779,.T.);
#6084=ORIENTED_EDGE('',*,*,#4775,.T.);
#6085=ORIENTED_EDGE('',*,*,#4805,.F.);
#6086=ORIENTED_EDGE('',*,*,#4797,.T.);
#6087=ORIENTED_EDGE('',*,*,#4795,.T.);
#6088=ORIENTED_EDGE('',*,*,#4793,.T.);
#6089=ORIENTED_EDGE('',*,*,#4791,.T.);
#6090=ORIENTED_EDGE('',*,*,#4789,.T.);
#6091=ORIENTED_EDGE('',*,*,#4806,.T.);
#6092=ORIENTED_EDGE('',*,*,#4807,.T.);
#6093=ORIENTED_EDGE('',*,*,#4808,.F.);
#6094=ORIENTED_EDGE('',*,*,#4809,.F.);
#6095=ORIENTED_EDGE('',*,*,#4810,.T.);
#6096=ORIENTED_EDGE('',*,*,#4809,.T.);
#6097=ORIENTED_EDGE('',*,*,#4811,.F.);
#6098=ORIENTED_EDGE('',*,*,#4812,.F.);
#6099=ORIENTED_EDGE('',*,*,#4813,.T.);
#6100=ORIENTED_EDGE('',*,*,#4812,.T.);
#6101=ORIENTED_EDGE('',*,*,#4814,.F.);
#6102=ORIENTED_EDGE('',*,*,#4815,.F.);
#6103=ORIENTED_EDGE('',*,*,#4816,.T.);
#6104=ORIENTED_EDGE('',*,*,#4815,.T.);
#6105=ORIENTED_EDGE('',*,*,#4817,.F.);
#6106=ORIENTED_EDGE('',*,*,#4807,.F.);
#6107=ORIENTED_EDGE('',*,*,#4817,.T.);
#6108=ORIENTED_EDGE('',*,*,#4814,.T.);
#6109=ORIENTED_EDGE('',*,*,#4811,.T.);
#6110=ORIENTED_EDGE('',*,*,#4808,.T.);
#6111=ORIENTED_EDGE('',*,*,#4816,.F.);
#6112=ORIENTED_EDGE('',*,*,#4806,.F.);
#6113=ORIENTED_EDGE('',*,*,#4810,.F.);
#6114=ORIENTED_EDGE('',*,*,#4813,.F.);
#6115=ORIENTED_EDGE('',*,*,#4818,.F.);
#6116=ORIENTED_EDGE('',*,*,#4819,.T.);
#6117=ORIENTED_EDGE('',*,*,#4820,.T.);
#6118=ORIENTED_EDGE('',*,*,#4819,.F.);
#6119=ORIENTED_EDGE('',*,*,#4820,.F.);
#6120=ORIENTED_EDGE('',*,*,#4821,.F.);
#6121=ORIENTED_EDGE('',*,*,#4822,.T.);
#6122=ORIENTED_EDGE('',*,*,#4823,.T.);
#6123=ORIENTED_EDGE('',*,*,#4822,.F.);
#6124=ORIENTED_EDGE('',*,*,#4823,.F.);
#6125=ORIENTED_EDGE('',*,*,#4824,.T.);
#6126=ORIENTED_EDGE('',*,*,#4825,.T.);
#6127=ORIENTED_EDGE('',*,*,#4826,.F.);
#6128=ORIENTED_EDGE('',*,*,#4827,.F.);
#6129=ORIENTED_EDGE('',*,*,#4828,.T.);
#6130=ORIENTED_EDGE('',*,*,#4827,.T.);
#6131=ORIENTED_EDGE('',*,*,#4829,.F.);
#6132=ORIENTED_EDGE('',*,*,#4830,.F.);
#6133=ORIENTED_EDGE('',*,*,#4831,.T.);
#6134=ORIENTED_EDGE('',*,*,#4830,.T.);
#6135=ORIENTED_EDGE('',*,*,#4832,.F.);
#6136=ORIENTED_EDGE('',*,*,#4833,.F.);
#6137=ORIENTED_EDGE('',*,*,#4834,.T.);
#6138=ORIENTED_EDGE('',*,*,#4833,.T.);
#6139=ORIENTED_EDGE('',*,*,#4835,.F.);
#6140=ORIENTED_EDGE('',*,*,#4825,.F.);
#6141=ORIENTED_EDGE('',*,*,#4835,.T.);
#6142=ORIENTED_EDGE('',*,*,#4832,.T.);
#6143=ORIENTED_EDGE('',*,*,#4829,.T.);
#6144=ORIENTED_EDGE('',*,*,#4826,.T.);
#6145=ORIENTED_EDGE('',*,*,#4834,.F.);
#6146=ORIENTED_EDGE('',*,*,#4824,.F.);
#6147=ORIENTED_EDGE('',*,*,#4828,.F.);
#6148=ORIENTED_EDGE('',*,*,#4831,.F.);
#6149=ORIENTED_EDGE('',*,*,#4818,.T.);
#6150=ORIENTED_EDGE('',*,*,#4821,.T.);
#6151=ORIENTED_EDGE('',*,*,#4836,.F.);
#6152=ORIENTED_EDGE('',*,*,#4837,.T.);
#6153=ORIENTED_EDGE('',*,*,#4838,.T.);
#6154=ORIENTED_EDGE('',*,*,#4837,.F.);
#6155=ORIENTED_EDGE('',*,*,#4838,.F.);
#6156=ORIENTED_EDGE('',*,*,#4839,.F.);
#6157=ORIENTED_EDGE('',*,*,#4840,.T.);
#6158=ORIENTED_EDGE('',*,*,#4841,.T.);
#6159=ORIENTED_EDGE('',*,*,#4840,.F.);
#6160=ORIENTED_EDGE('',*,*,#4841,.F.);
#6161=ORIENTED_EDGE('',*,*,#4842,.T.);
#6162=ORIENTED_EDGE('',*,*,#4843,.T.);
#6163=ORIENTED_EDGE('',*,*,#4844,.F.);
#6164=ORIENTED_EDGE('',*,*,#4845,.F.);
#6165=ORIENTED_EDGE('',*,*,#4846,.T.);
#6166=ORIENTED_EDGE('',*,*,#4845,.T.);
#6167=ORIENTED_EDGE('',*,*,#4847,.F.);
#6168=ORIENTED_EDGE('',*,*,#4848,.F.);
#6169=ORIENTED_EDGE('',*,*,#4849,.T.);
#6170=ORIENTED_EDGE('',*,*,#4848,.T.);
#6171=ORIENTED_EDGE('',*,*,#4850,.F.);
#6172=ORIENTED_EDGE('',*,*,#4851,.F.);
#6173=ORIENTED_EDGE('',*,*,#4852,.T.);
#6174=ORIENTED_EDGE('',*,*,#4851,.T.);
#6175=ORIENTED_EDGE('',*,*,#4853,.F.);
#6176=ORIENTED_EDGE('',*,*,#4843,.F.);
#6177=ORIENTED_EDGE('',*,*,#4853,.T.);
#6178=ORIENTED_EDGE('',*,*,#4850,.T.);
#6179=ORIENTED_EDGE('',*,*,#4847,.T.);
#6180=ORIENTED_EDGE('',*,*,#4844,.T.);
#6181=ORIENTED_EDGE('',*,*,#4852,.F.);
#6182=ORIENTED_EDGE('',*,*,#4842,.F.);
#6183=ORIENTED_EDGE('',*,*,#4846,.F.);
#6184=ORIENTED_EDGE('',*,*,#4849,.F.);
#6185=ORIENTED_EDGE('',*,*,#4836,.T.);
#6186=ORIENTED_EDGE('',*,*,#4839,.T.);
#6187=ORIENTED_EDGE('',*,*,#4854,.F.);
#6188=ORIENTED_EDGE('',*,*,#4855,.T.);
#6189=ORIENTED_EDGE('',*,*,#4856,.F.);
#6190=ORIENTED_EDGE('',*,*,#4855,.F.);
#6191=ORIENTED_EDGE('',*,*,#4854,.T.);
#6192=ORIENTED_EDGE('',*,*,#4857,.F.);
#6193=ORIENTED_EDGE('',*,*,#4858,.T.);
#6194=ORIENTED_EDGE('',*,*,#4859,.F.);
#6195=ORIENTED_EDGE('',*,*,#4860,.T.);
#6196=ORIENTED_EDGE('',*,*,#4857,.T.);
#6197=ORIENTED_EDGE('',*,*,#4860,.F.);
#6198=ORIENTED_EDGE('',*,*,#4859,.T.);
#6199=ORIENTED_EDGE('',*,*,#4856,.T.);
#6200=ORIENTED_EDGE('',*,*,#4858,.F.);
#6201=ORIENTED_EDGE('',*,*,#4861,.T.);
#6202=ORIENTED_EDGE('',*,*,#4862,.T.);
#6203=ORIENTED_EDGE('',*,*,#4861,.F.);
#6204=ORIENTED_EDGE('',*,*,#4862,.F.);
#6205=ORIENTED_EDGE('',*,*,#4863,.F.);
#6206=ORIENTED_EDGE('',*,*,#4864,.T.);
#6207=ORIENTED_EDGE('',*,*,#4865,.F.);
#6208=ORIENTED_EDGE('',*,*,#4866,.F.);
#6209=ORIENTED_EDGE('',*,*,#4867,.F.);
#6210=ORIENTED_EDGE('',*,*,#4868,.T.);
#6211=ORIENTED_EDGE('',*,*,#4869,.F.);
#6212=ORIENTED_EDGE('',*,*,#4864,.F.);
#6213=ORIENTED_EDGE('',*,*,#4870,.F.);
#6214=ORIENTED_EDGE('',*,*,#4871,.T.);
#6215=ORIENTED_EDGE('',*,*,#4872,.F.);
#6216=ORIENTED_EDGE('',*,*,#4868,.F.);
#6217=ORIENTED_EDGE('',*,*,#4873,.F.);
#6218=ORIENTED_EDGE('',*,*,#4874,.T.);
#6219=ORIENTED_EDGE('',*,*,#4875,.F.);
#6220=ORIENTED_EDGE('',*,*,#4871,.F.);
#6221=ORIENTED_EDGE('',*,*,#4876,.F.);
#6222=ORIENTED_EDGE('',*,*,#4877,.T.);
#6223=ORIENTED_EDGE('',*,*,#4878,.F.);
#6224=ORIENTED_EDGE('',*,*,#4874,.F.);
#6225=ORIENTED_EDGE('',*,*,#4879,.F.);
#6226=ORIENTED_EDGE('',*,*,#4880,.T.);
#6227=ORIENTED_EDGE('',*,*,#4881,.F.);
#6228=ORIENTED_EDGE('',*,*,#4877,.F.);
#6229=ORIENTED_EDGE('',*,*,#4882,.F.);
#6230=ORIENTED_EDGE('',*,*,#4883,.T.);
#6231=ORIENTED_EDGE('',*,*,#4884,.F.);
#6232=ORIENTED_EDGE('',*,*,#4880,.F.);
#6233=ORIENTED_EDGE('',*,*,#4885,.F.);
#6234=ORIENTED_EDGE('',*,*,#4886,.T.);
#6235=ORIENTED_EDGE('',*,*,#4887,.F.);
#6236=ORIENTED_EDGE('',*,*,#4883,.F.);
#6237=ORIENTED_EDGE('',*,*,#4888,.F.);
#6238=ORIENTED_EDGE('',*,*,#4889,.F.);
#6239=ORIENTED_EDGE('',*,*,#4890,.F.);
#6240=ORIENTED_EDGE('',*,*,#4886,.F.);
#6241=ORIENTED_EDGE('',*,*,#4891,.F.);
#6242=ORIENTED_EDGE('',*,*,#4892,.T.);
#6243=ORIENTED_EDGE('',*,*,#4893,.F.);
#6244=ORIENTED_EDGE('',*,*,#4894,.F.);
#6245=ORIENTED_EDGE('',*,*,#4895,.F.);
#6246=ORIENTED_EDGE('',*,*,#4896,.T.);
#6247=ORIENTED_EDGE('',*,*,#4897,.F.);
#6248=ORIENTED_EDGE('',*,*,#4892,.F.);
#6249=ORIENTED_EDGE('',*,*,#4898,.F.);
#6250=ORIENTED_EDGE('',*,*,#4899,.T.);
#6251=ORIENTED_EDGE('',*,*,#4900,.F.);
#6252=ORIENTED_EDGE('',*,*,#4896,.F.);
#6253=ORIENTED_EDGE('',*,*,#4901,.F.);
#6254=ORIENTED_EDGE('',*,*,#4902,.T.);
#6255=ORIENTED_EDGE('',*,*,#4903,.F.);
#6256=ORIENTED_EDGE('',*,*,#4899,.F.);
#6257=ORIENTED_EDGE('',*,*,#4904,.F.);
#6258=ORIENTED_EDGE('',*,*,#4905,.T.);
#6259=ORIENTED_EDGE('',*,*,#4906,.F.);
#6260=ORIENTED_EDGE('',*,*,#4902,.F.);
#6261=ORIENTED_EDGE('',*,*,#4907,.F.);
#6262=ORIENTED_EDGE('',*,*,#4908,.T.);
#6263=ORIENTED_EDGE('',*,*,#4909,.F.);
#6264=ORIENTED_EDGE('',*,*,#4905,.F.);
#6265=ORIENTED_EDGE('',*,*,#4910,.F.);
#6266=ORIENTED_EDGE('',*,*,#4911,.T.);
#6267=ORIENTED_EDGE('',*,*,#4912,.F.);
#6268=ORIENTED_EDGE('',*,*,#4908,.F.);
#6269=ORIENTED_EDGE('',*,*,#4913,.F.);
#6270=ORIENTED_EDGE('',*,*,#4914,.T.);
#6271=ORIENTED_EDGE('',*,*,#4915,.F.);
#6272=ORIENTED_EDGE('',*,*,#4911,.F.);
#6273=ORIENTED_EDGE('',*,*,#4916,.F.);
#6274=ORIENTED_EDGE('',*,*,#4917,.F.);
#6275=ORIENTED_EDGE('',*,*,#4918,.F.);
#6276=ORIENTED_EDGE('',*,*,#4914,.F.);
#6277=ORIENTED_EDGE('',*,*,#4919,.F.);
#6278=ORIENTED_EDGE('',*,*,#4920,.T.);
#6279=ORIENTED_EDGE('',*,*,#4921,.F.);
#6280=ORIENTED_EDGE('',*,*,#4922,.F.);
#6281=ORIENTED_EDGE('',*,*,#4923,.F.);
#6282=ORIENTED_EDGE('',*,*,#4924,.T.);
#6283=ORIENTED_EDGE('',*,*,#4925,.F.);
#6284=ORIENTED_EDGE('',*,*,#4920,.F.);
#6285=ORIENTED_EDGE('',*,*,#4926,.F.);
#6286=ORIENTED_EDGE('',*,*,#4927,.T.);
#6287=ORIENTED_EDGE('',*,*,#4928,.F.);
#6288=ORIENTED_EDGE('',*,*,#4924,.F.);
#6289=ORIENTED_EDGE('',*,*,#4929,.F.);
#6290=ORIENTED_EDGE('',*,*,#4930,.T.);
#6291=ORIENTED_EDGE('',*,*,#4931,.F.);
#6292=ORIENTED_EDGE('',*,*,#4927,.F.);
#6293=ORIENTED_EDGE('',*,*,#4932,.F.);
#6294=ORIENTED_EDGE('',*,*,#4933,.T.);
#6295=ORIENTED_EDGE('',*,*,#4934,.F.);
#6296=ORIENTED_EDGE('',*,*,#4930,.F.);
#6297=ORIENTED_EDGE('',*,*,#4935,.F.);
#6298=ORIENTED_EDGE('',*,*,#4936,.T.);
#6299=ORIENTED_EDGE('',*,*,#4937,.F.);
#6300=ORIENTED_EDGE('',*,*,#4933,.F.);
#6301=ORIENTED_EDGE('',*,*,#4938,.F.);
#6302=ORIENTED_EDGE('',*,*,#4939,.T.);
#6303=ORIENTED_EDGE('',*,*,#4940,.F.);
#6304=ORIENTED_EDGE('',*,*,#4936,.F.);
#6305=ORIENTED_EDGE('',*,*,#4941,.F.);
#6306=ORIENTED_EDGE('',*,*,#4942,.T.);
#6307=ORIENTED_EDGE('',*,*,#4943,.F.);
#6308=ORIENTED_EDGE('',*,*,#4939,.F.);
#6309=ORIENTED_EDGE('',*,*,#4944,.F.);
#6310=ORIENTED_EDGE('',*,*,#4945,.F.);
#6311=ORIENTED_EDGE('',*,*,#4946,.F.);
#6312=ORIENTED_EDGE('',*,*,#4942,.F.);
#6313=ORIENTED_EDGE('',*,*,#4947,.F.);
#6314=ORIENTED_EDGE('',*,*,#4948,.T.);
#6315=ORIENTED_EDGE('',*,*,#4949,.F.);
#6316=ORIENTED_EDGE('',*,*,#4950,.F.);
#6317=ORIENTED_EDGE('',*,*,#4951,.F.);
#6318=ORIENTED_EDGE('',*,*,#4952,.T.);
#6319=ORIENTED_EDGE('',*,*,#4953,.F.);
#6320=ORIENTED_EDGE('',*,*,#4948,.F.);
#6321=ORIENTED_EDGE('',*,*,#4954,.F.);
#6322=ORIENTED_EDGE('',*,*,#4955,.T.);
#6323=ORIENTED_EDGE('',*,*,#4956,.F.);
#6324=ORIENTED_EDGE('',*,*,#4952,.F.);
#6325=ORIENTED_EDGE('',*,*,#4957,.F.);
#6326=ORIENTED_EDGE('',*,*,#4958,.T.);
#6327=ORIENTED_EDGE('',*,*,#4959,.F.);
#6328=ORIENTED_EDGE('',*,*,#4955,.F.);
#6329=ORIENTED_EDGE('',*,*,#4960,.F.);
#6330=ORIENTED_EDGE('',*,*,#4961,.T.);
#6331=ORIENTED_EDGE('',*,*,#4962,.F.);
#6332=ORIENTED_EDGE('',*,*,#4958,.F.);
#6333=ORIENTED_EDGE('',*,*,#4963,.F.);
#6334=ORIENTED_EDGE('',*,*,#4964,.T.);
#6335=ORIENTED_EDGE('',*,*,#4965,.F.);
#6336=ORIENTED_EDGE('',*,*,#4961,.F.);
#6337=ORIENTED_EDGE('',*,*,#4966,.F.);
#6338=ORIENTED_EDGE('',*,*,#4967,.T.);
#6339=ORIENTED_EDGE('',*,*,#4968,.F.);
#6340=ORIENTED_EDGE('',*,*,#4964,.F.);
#6341=ORIENTED_EDGE('',*,*,#4969,.F.);
#6342=ORIENTED_EDGE('',*,*,#4970,.T.);
#6343=ORIENTED_EDGE('',*,*,#4971,.F.);
#6344=ORIENTED_EDGE('',*,*,#4967,.F.);
#6345=ORIENTED_EDGE('',*,*,#4972,.F.);
#6346=ORIENTED_EDGE('',*,*,#4973,.F.);
#6347=ORIENTED_EDGE('',*,*,#4974,.F.);
#6348=ORIENTED_EDGE('',*,*,#4970,.F.);
#6349=ORIENTED_EDGE('',*,*,#4975,.F.);
#6350=ORIENTED_EDGE('',*,*,#4976,.T.);
#6351=ORIENTED_EDGE('',*,*,#4977,.F.);
#6352=ORIENTED_EDGE('',*,*,#4976,.F.);
#6353=ORIENTED_EDGE('',*,*,#4889,.T.);
#6354=ORIENTED_EDGE('',*,*,#4978,.T.);
#6355=ORIENTED_EDGE('',*,*,#4979,.T.);
#6356=ORIENTED_EDGE('',*,*,#4980,.F.);
#6357=ORIENTED_EDGE('',*,*,#4866,.T.);
#6358=ORIENTED_EDGE('',*,*,#4981,.F.);
#6359=ORIENTED_EDGE('',*,*,#4982,.F.);
#6360=ORIENTED_EDGE('',*,*,#4983,.T.);
#6361=ORIENTED_EDGE('',*,*,#4917,.T.);
#6362=ORIENTED_EDGE('',*,*,#4984,.T.);
#6363=ORIENTED_EDGE('',*,*,#4982,.T.);
#6364=ORIENTED_EDGE('',*,*,#4985,.F.);
#6365=ORIENTED_EDGE('',*,*,#4894,.T.);
#6366=ORIENTED_EDGE('',*,*,#4986,.F.);
#6367=ORIENTED_EDGE('',*,*,#4987,.F.);
#6368=ORIENTED_EDGE('',*,*,#4988,.T.);
#6369=ORIENTED_EDGE('',*,*,#4945,.T.);
#6370=ORIENTED_EDGE('',*,*,#4989,.T.);
#6371=ORIENTED_EDGE('',*,*,#4987,.T.);
#6372=ORIENTED_EDGE('',*,*,#4990,.F.);
#6373=ORIENTED_EDGE('',*,*,#4922,.T.);
#6374=ORIENTED_EDGE('',*,*,#4991,.F.);
#6375=ORIENTED_EDGE('',*,*,#4992,.F.);
#6376=ORIENTED_EDGE('',*,*,#4993,.T.);
#6377=ORIENTED_EDGE('',*,*,#4973,.T.);
#6378=ORIENTED_EDGE('',*,*,#4994,.T.);
#6379=ORIENTED_EDGE('',*,*,#4992,.T.);
#6380=ORIENTED_EDGE('',*,*,#4995,.F.);
#6381=ORIENTED_EDGE('',*,*,#4950,.T.);
#6382=ORIENTED_EDGE('',*,*,#4996,.F.);
#6383=ORIENTED_EDGE('',*,*,#4979,.F.);
#6384=ORIENTED_EDGE('',*,*,#4997,.T.);
#6385=ORIENTED_EDGE('',*,*,#4865,.T.);
#6386=ORIENTED_EDGE('',*,*,#4869,.T.);
#6387=ORIENTED_EDGE('',*,*,#4872,.T.);
#6388=ORIENTED_EDGE('',*,*,#4875,.T.);
#6389=ORIENTED_EDGE('',*,*,#4878,.T.);
#6390=ORIENTED_EDGE('',*,*,#4881,.T.);
#6391=ORIENTED_EDGE('',*,*,#4884,.T.);
#6392=ORIENTED_EDGE('',*,*,#4887,.T.);
#6393=ORIENTED_EDGE('',*,*,#4890,.T.);
#6394=ORIENTED_EDGE('',*,*,#4980,.T.);
#6395=ORIENTED_EDGE('',*,*,#4996,.T.);
#6396=ORIENTED_EDGE('',*,*,#4949,.T.);
#6397=ORIENTED_EDGE('',*,*,#4953,.T.);
#6398=ORIENTED_EDGE('',*,*,#4956,.T.);
#6399=ORIENTED_EDGE('',*,*,#4959,.T.);
#6400=ORIENTED_EDGE('',*,*,#4962,.T.);
#6401=ORIENTED_EDGE('',*,*,#4965,.T.);
#6402=ORIENTED_EDGE('',*,*,#4968,.T.);
#6403=ORIENTED_EDGE('',*,*,#4971,.T.);
#6404=ORIENTED_EDGE('',*,*,#4974,.T.);
#6405=ORIENTED_EDGE('',*,*,#4995,.T.);
#6406=ORIENTED_EDGE('',*,*,#4991,.T.);
#6407=ORIENTED_EDGE('',*,*,#4921,.T.);
#6408=ORIENTED_EDGE('',*,*,#4925,.T.);
#6409=ORIENTED_EDGE('',*,*,#4928,.T.);
#6410=ORIENTED_EDGE('',*,*,#4931,.T.);
#6411=ORIENTED_EDGE('',*,*,#4934,.T.);
#6412=ORIENTED_EDGE('',*,*,#4937,.T.);
#6413=ORIENTED_EDGE('',*,*,#4940,.T.);
#6414=ORIENTED_EDGE('',*,*,#4943,.T.);
#6415=ORIENTED_EDGE('',*,*,#4946,.T.);
#6416=ORIENTED_EDGE('',*,*,#4990,.T.);
#6417=ORIENTED_EDGE('',*,*,#4986,.T.);
#6418=ORIENTED_EDGE('',*,*,#4893,.T.);
#6419=ORIENTED_EDGE('',*,*,#4897,.T.);
#6420=ORIENTED_EDGE('',*,*,#4900,.T.);
#6421=ORIENTED_EDGE('',*,*,#4903,.T.);
#6422=ORIENTED_EDGE('',*,*,#4906,.T.);
#6423=ORIENTED_EDGE('',*,*,#4909,.T.);
#6424=ORIENTED_EDGE('',*,*,#4912,.T.);
#6425=ORIENTED_EDGE('',*,*,#4915,.T.);
#6426=ORIENTED_EDGE('',*,*,#4918,.T.);
#6427=ORIENTED_EDGE('',*,*,#4985,.T.);
#6428=ORIENTED_EDGE('',*,*,#4981,.T.);
#6429=ORIENTED_EDGE('',*,*,#4977,.T.);
#6430=ORIENTED_EDGE('',*,*,#4863,.T.);
#6431=ORIENTED_EDGE('',*,*,#4983,.F.);
#6432=ORIENTED_EDGE('',*,*,#4984,.F.);
#6433=ORIENTED_EDGE('',*,*,#4916,.T.);
#6434=ORIENTED_EDGE('',*,*,#4913,.T.);
#6435=ORIENTED_EDGE('',*,*,#4910,.T.);
#6436=ORIENTED_EDGE('',*,*,#4907,.T.);
#6437=ORIENTED_EDGE('',*,*,#4904,.T.);
#6438=ORIENTED_EDGE('',*,*,#4901,.T.);
#6439=ORIENTED_EDGE('',*,*,#4898,.T.);
#6440=ORIENTED_EDGE('',*,*,#4895,.T.);
#6441=ORIENTED_EDGE('',*,*,#4891,.T.);
#6442=ORIENTED_EDGE('',*,*,#4988,.F.);
#6443=ORIENTED_EDGE('',*,*,#4989,.F.);
#6444=ORIENTED_EDGE('',*,*,#4944,.T.);
#6445=ORIENTED_EDGE('',*,*,#4941,.T.);
#6446=ORIENTED_EDGE('',*,*,#4938,.T.);
#6447=ORIENTED_EDGE('',*,*,#4935,.T.);
#6448=ORIENTED_EDGE('',*,*,#4932,.T.);
#6449=ORIENTED_EDGE('',*,*,#4929,.T.);
#6450=ORIENTED_EDGE('',*,*,#4926,.T.);
#6451=ORIENTED_EDGE('',*,*,#4923,.T.);
#6452=ORIENTED_EDGE('',*,*,#4919,.T.);
#6453=ORIENTED_EDGE('',*,*,#4993,.F.);
#6454=ORIENTED_EDGE('',*,*,#4994,.F.);
#6455=ORIENTED_EDGE('',*,*,#4972,.T.);
#6456=ORIENTED_EDGE('',*,*,#4969,.T.);
#6457=ORIENTED_EDGE('',*,*,#4966,.T.);
#6458=ORIENTED_EDGE('',*,*,#4963,.T.);
#6459=ORIENTED_EDGE('',*,*,#4960,.T.);
#6460=ORIENTED_EDGE('',*,*,#4957,.T.);
#6461=ORIENTED_EDGE('',*,*,#4954,.T.);
#6462=ORIENTED_EDGE('',*,*,#4951,.T.);
#6463=ORIENTED_EDGE('',*,*,#4947,.T.);
#6464=ORIENTED_EDGE('',*,*,#4997,.F.);
#6465=ORIENTED_EDGE('',*,*,#4978,.F.);
#6466=ORIENTED_EDGE('',*,*,#4888,.T.);
#6467=ORIENTED_EDGE('',*,*,#4885,.T.);
#6468=ORIENTED_EDGE('',*,*,#4882,.T.);
#6469=ORIENTED_EDGE('',*,*,#4879,.T.);
#6470=ORIENTED_EDGE('',*,*,#4876,.T.);
#6471=ORIENTED_EDGE('',*,*,#4873,.T.);
#6472=ORIENTED_EDGE('',*,*,#4870,.T.);
#6473=ORIENTED_EDGE('',*,*,#4867,.T.);
#6474=ORIENTED_EDGE('',*,*,#4975,.T.);
#6475=ORIENTED_EDGE('',*,*,#4998,.F.);
#6476=ORIENTED_EDGE('',*,*,#4999,.F.);
#6477=ORIENTED_EDGE('',*,*,#5000,.F.);
#6478=ORIENTED_EDGE('',*,*,#5001,.F.);
#6479=ORIENTED_EDGE('',*,*,#5000,.T.);
#6480=ORIENTED_EDGE('',*,*,#5002,.T.);
#6481=ORIENTED_EDGE('',*,*,#5003,.F.);
#6482=ORIENTED_EDGE('',*,*,#5004,.F.);
#6483=ORIENTED_EDGE('',*,*,#5005,.T.);
#6484=ORIENTED_EDGE('',*,*,#5006,.T.);
#6485=ORIENTED_EDGE('',*,*,#5007,.T.);
#6486=ORIENTED_EDGE('',*,*,#5003,.T.);
#6487=ORIENTED_EDGE('',*,*,#5008,.T.);
#6488=ORIENTED_EDGE('',*,*,#5005,.F.);
#6489=ORIENTED_EDGE('',*,*,#5002,.F.);
#6490=ORIENTED_EDGE('',*,*,#4999,.T.);
#6491=ORIENTED_EDGE('',*,*,#5009,.F.);
#6492=ORIENTED_EDGE('',*,*,#5010,.F.);
#6493=ORIENTED_EDGE('',*,*,#5011,.T.);
#6494=ORIENTED_EDGE('',*,*,#5012,.F.);
#6495=ORIENTED_EDGE('',*,*,#5013,.T.);
#6496=ORIENTED_EDGE('',*,*,#5014,.T.);
#6497=ORIENTED_EDGE('',*,*,#5015,.T.);
#6498=ORIENTED_EDGE('',*,*,#5016,.T.);
#6499=ORIENTED_EDGE('',*,*,#5017,.T.);
#6500=ORIENTED_EDGE('',*,*,#5006,.F.);
#6501=ORIENTED_EDGE('',*,*,#5015,.F.);
#6502=ORIENTED_EDGE('',*,*,#5018,.F.);
#6503=ORIENTED_EDGE('',*,*,#5019,.F.);
#6504=ORIENTED_EDGE('',*,*,#5016,.F.);
#6505=ORIENTED_EDGE('',*,*,#5014,.F.);
#6506=ORIENTED_EDGE('',*,*,#5007,.F.);
#6507=ORIENTED_EDGE('',*,*,#5017,.F.);
#6508=ORIENTED_EDGE('',*,*,#5019,.T.);
#6509=ORIENTED_EDGE('',*,*,#5020,.F.);
#6510=ORIENTED_EDGE('',*,*,#5021,.F.);
#6511=ORIENTED_EDGE('',*,*,#5022,.T.);
#6512=ORIENTED_EDGE('',*,*,#5023,.F.);
#6513=ORIENTED_EDGE('',*,*,#5024,.T.);
#6514=ORIENTED_EDGE('',*,*,#5001,.T.);
#6515=ORIENTED_EDGE('',*,*,#5004,.T.);
#6516=ORIENTED_EDGE('',*,*,#5018,.T.);
#6517=ORIENTED_EDGE('',*,*,#5013,.F.);
#6518=ORIENTED_EDGE('',*,*,#5025,.F.);
#6519=ORIENTED_EDGE('',*,*,#5020,.T.);
#6520=ORIENTED_EDGE('',*,*,#5021,.T.);
#6521=ORIENTED_EDGE('',*,*,#5025,.T.);
#6522=ORIENTED_EDGE('',*,*,#5012,.T.);
#6523=ORIENTED_EDGE('',*,*,#5026,.T.);
#6524=ORIENTED_EDGE('',*,*,#5027,.T.);
#6525=ORIENTED_EDGE('',*,*,#5028,.T.);
#6526=ORIENTED_EDGE('',*,*,#5027,.F.);
#6527=ORIENTED_EDGE('',*,*,#5029,.F.);
#6528=ORIENTED_EDGE('',*,*,#5030,.T.);
#6529=ORIENTED_EDGE('',*,*,#5008,.F.);
#6530=ORIENTED_EDGE('',*,*,#5030,.F.);
#6531=ORIENTED_EDGE('',*,*,#5031,.F.);
#6532=ORIENTED_EDGE('',*,*,#5032,.F.);
#6533=ORIENTED_EDGE('',*,*,#5033,.F.);
#6534=ORIENTED_EDGE('',*,*,#5026,.F.);
#6535=ORIENTED_EDGE('',*,*,#5011,.F.);
#6536=ORIENTED_EDGE('',*,*,#5034,.F.);
#6537=ORIENTED_EDGE('',*,*,#5031,.T.);
#6538=ORIENTED_EDGE('',*,*,#5029,.T.);
#6539=ORIENTED_EDGE('',*,*,#5028,.F.);
#6540=ORIENTED_EDGE('',*,*,#5033,.T.);
#6541=ORIENTED_EDGE('',*,*,#5035,.F.);
#6542=ORIENTED_EDGE('',*,*,#5022,.F.);
#6543=ORIENTED_EDGE('',*,*,#5010,.T.);
#6544=ORIENTED_EDGE('',*,*,#5036,.T.);
#6545=ORIENTED_EDGE('',*,*,#5023,.T.);
#6546=ORIENTED_EDGE('',*,*,#5035,.T.);
#6547=ORIENTED_EDGE('',*,*,#5032,.T.);
#6548=ORIENTED_EDGE('',*,*,#5034,.T.);
#6549=ORIENTED_EDGE('',*,*,#4998,.T.);
#6550=ORIENTED_EDGE('',*,*,#5024,.F.);
#6551=ORIENTED_EDGE('',*,*,#5036,.F.);
#6552=ORIENTED_EDGE('',*,*,#5009,.T.);
#6553=ORIENTED_EDGE('',*,*,#5037,.T.);
#6554=ORIENTED_EDGE('',*,*,#5038,.T.);
#6555=ORIENTED_EDGE('',*,*,#5039,.T.);
#6556=ORIENTED_EDGE('',*,*,#5038,.F.);
#6557=ORIENTED_EDGE('',*,*,#5039,.F.);
#6558=ORIENTED_EDGE('',*,*,#5040,.T.);
#6559=ORIENTED_EDGE('',*,*,#5041,.T.);
#6560=ORIENTED_EDGE('',*,*,#5040,.F.);
#6561=ORIENTED_EDGE('',*,*,#5042,.T.);
#6562=ORIENTED_EDGE('',*,*,#5037,.F.);
#6563=ORIENTED_EDGE('',*,*,#5042,.F.);
#6564=ORIENTED_EDGE('',*,*,#5043,.T.);
#6565=ORIENTED_EDGE('',*,*,#5044,.T.);
#6566=ORIENTED_EDGE('',*,*,#5043,.F.);
#6567=ORIENTED_EDGE('',*,*,#5044,.F.);
#6568=ORIENTED_EDGE('',*,*,#5041,.F.);
#6569=ORIENTED_EDGE('',*,*,#5045,.T.);
#6570=ORIENTED_EDGE('',*,*,#5046,.T.);
#6571=ORIENTED_EDGE('',*,*,#5047,.T.);
#6572=ORIENTED_EDGE('',*,*,#5048,.F.);
#6573=ORIENTED_EDGE('',*,*,#5049,.T.);
#6574=ORIENTED_EDGE('',*,*,#5050,.T.);
#6575=ORIENTED_EDGE('',*,*,#5051,.T.);
#6576=ORIENTED_EDGE('',*,*,#5046,.F.);
#6577=ORIENTED_EDGE('',*,*,#5052,.T.);
#6578=ORIENTED_EDGE('',*,*,#5053,.T.);
#6579=ORIENTED_EDGE('',*,*,#5054,.T.);
#6580=ORIENTED_EDGE('',*,*,#5050,.F.);
#6581=ORIENTED_EDGE('',*,*,#5055,.T.);
#6582=ORIENTED_EDGE('',*,*,#5056,.T.);
#6583=ORIENTED_EDGE('',*,*,#5057,.T.);
#6584=ORIENTED_EDGE('',*,*,#5053,.F.);
#6585=ORIENTED_EDGE('',*,*,#5058,.T.);
#6586=ORIENTED_EDGE('',*,*,#5059,.T.);
#6587=ORIENTED_EDGE('',*,*,#5060,.T.);
#6588=ORIENTED_EDGE('',*,*,#5056,.F.);
#6589=ORIENTED_EDGE('',*,*,#5061,.T.);
#6590=ORIENTED_EDGE('',*,*,#5048,.T.);
#6591=ORIENTED_EDGE('',*,*,#5062,.T.);
#6592=ORIENTED_EDGE('',*,*,#5059,.F.);
#6593=ORIENTED_EDGE('',*,*,#5061,.F.);
#6594=ORIENTED_EDGE('',*,*,#5058,.F.);
#6595=ORIENTED_EDGE('',*,*,#5055,.F.);
#6596=ORIENTED_EDGE('',*,*,#5052,.F.);
#6597=ORIENTED_EDGE('',*,*,#5049,.F.);
#6598=ORIENTED_EDGE('',*,*,#5045,.F.);
#6599=ORIENTED_EDGE('',*,*,#5062,.F.);
#6600=ORIENTED_EDGE('',*,*,#5047,.F.);
#6601=ORIENTED_EDGE('',*,*,#5051,.F.);
#6602=ORIENTED_EDGE('',*,*,#5054,.F.);
#6603=ORIENTED_EDGE('',*,*,#5057,.F.);
#6604=ORIENTED_EDGE('',*,*,#5060,.F.);
#6605=ORIENTED_EDGE('',*,*,#5063,.F.);
#6606=ORIENTED_EDGE('',*,*,#5064,.F.);
#6607=ORIENTED_EDGE('',*,*,#5065,.F.);
#6608=ORIENTED_EDGE('',*,*,#5066,.T.);
#6609=ORIENTED_EDGE('',*,*,#5064,.T.);
#6610=ORIENTED_EDGE('',*,*,#5066,.F.);
#6611=ORIENTED_EDGE('',*,*,#5067,.F.);
#6612=ORIENTED_EDGE('',*,*,#5068,.T.);
#6613=ORIENTED_EDGE('',*,*,#5065,.T.);
#6614=ORIENTED_EDGE('',*,*,#5068,.F.);
#6615=ORIENTED_EDGE('',*,*,#5069,.F.);
#6616=ORIENTED_EDGE('',*,*,#5070,.T.);
#6617=ORIENTED_EDGE('',*,*,#5067,.T.);
#6618=ORIENTED_EDGE('',*,*,#5070,.F.);
#6619=ORIENTED_EDGE('',*,*,#5069,.T.);
#6620=ORIENTED_EDGE('',*,*,#5071,.F.);
#6621=ORIENTED_EDGE('',*,*,#5072,.F.);
#6622=ORIENTED_EDGE('',*,*,#5073,.T.);
#6623=ORIENTED_EDGE('',*,*,#5071,.T.);
#6624=ORIENTED_EDGE('',*,*,#5073,.F.);
#6625=ORIENTED_EDGE('',*,*,#5063,.T.);
#6626=ORIENTED_EDGE('',*,*,#5074,.T.);
#6627=ORIENTED_EDGE('',*,*,#5072,.T.);
#6628=ORIENTED_EDGE('',*,*,#5074,.F.);
#6629=ORIENTED_EDGE('',*,*,#5075,.F.);
#6630=ORIENTED_EDGE('',*,*,#5076,.F.);
#6631=ORIENTED_EDGE('',*,*,#5077,.T.);
#6632=ORIENTED_EDGE('',*,*,#5078,.F.);
#6633=ORIENTED_EDGE('',*,*,#5079,.F.);
#6634=ORIENTED_EDGE('',*,*,#5077,.F.);
#6635=ORIENTED_EDGE('',*,*,#5078,.T.);
#6636=ORIENTED_EDGE('',*,*,#5079,.T.);
#6637=ORIENTED_EDGE('',*,*,#5080,.T.);
#6638=ORIENTED_EDGE('',*,*,#5081,.T.);
#6639=ORIENTED_EDGE('',*,*,#5080,.F.);
#6640=ORIENTED_EDGE('',*,*,#5082,.T.);
#6641=ORIENTED_EDGE('',*,*,#5083,.T.);
#6642=ORIENTED_EDGE('',*,*,#5084,.F.);
#6643=ORIENTED_EDGE('',*,*,#5083,.F.);
#6644=ORIENTED_EDGE('',*,*,#5084,.T.);
#6645=ORIENTED_EDGE('',*,*,#5085,.T.);
#6646=ORIENTED_EDGE('',*,*,#5086,.F.);
#6647=ORIENTED_EDGE('',*,*,#5085,.F.);
#6648=ORIENTED_EDGE('',*,*,#5081,.F.);
#6649=ORIENTED_EDGE('',*,*,#5086,.T.);
#6650=ORIENTED_EDGE('',*,*,#5087,.F.);
#6651=ORIENTED_EDGE('',*,*,#5088,.T.);
#6652=ORIENTED_EDGE('',*,*,#5075,.T.);
#6653=ORIENTED_EDGE('',*,*,#5076,.T.);
#6654=ORIENTED_EDGE('',*,*,#5088,.F.);
#6655=ORIENTED_EDGE('',*,*,#5087,.T.);
#6656=ORIENTED_EDGE('',*,*,#5089,.F.);
#6657=ORIENTED_EDGE('',*,*,#5089,.T.);
#6658=ORIENTED_EDGE('',*,*,#5090,.T.);
#6659=ORIENTED_EDGE('',*,*,#5082,.F.);
#6660=ORIENTED_EDGE('',*,*,#5090,.F.);
#6661=ORIENTED_EDGE('',*,*,#5091,.F.);
#6662=ORIENTED_EDGE('',*,*,#5092,.F.);
#6663=ORIENTED_EDGE('',*,*,#5093,.T.);
#6664=ORIENTED_EDGE('',*,*,#5094,.F.);
#6665=ORIENTED_EDGE('',*,*,#5095,.F.);
#6666=ORIENTED_EDGE('',*,*,#5093,.F.);
#6667=ORIENTED_EDGE('',*,*,#5096,.T.);
#6668=ORIENTED_EDGE('',*,*,#5097,.T.);
#6669=ORIENTED_EDGE('',*,*,#5094,.T.);
#6670=ORIENTED_EDGE('',*,*,#5095,.T.);
#6671=ORIENTED_EDGE('',*,*,#5097,.F.);
#6672=ORIENTED_EDGE('',*,*,#5098,.F.);
#6673=ORIENTED_EDGE('',*,*,#5099,.T.);
#6674=ORIENTED_EDGE('',*,*,#5100,.F.);
#6675=ORIENTED_EDGE('',*,*,#5101,.T.);
#6676=ORIENTED_EDGE('',*,*,#5098,.T.);
#6677=ORIENTED_EDGE('',*,*,#5101,.F.);
#6678=ORIENTED_EDGE('',*,*,#5102,.F.);
#6679=ORIENTED_EDGE('',*,*,#5103,.T.);
#6680=ORIENTED_EDGE('',*,*,#5100,.T.);
#6681=ORIENTED_EDGE('',*,*,#5103,.F.);
#6682=ORIENTED_EDGE('',*,*,#5104,.F.);
#6683=ORIENTED_EDGE('',*,*,#5105,.T.);
#6684=ORIENTED_EDGE('',*,*,#5102,.T.);
#6685=ORIENTED_EDGE('',*,*,#5105,.F.);
#6686=ORIENTED_EDGE('',*,*,#5104,.T.);
#6687=ORIENTED_EDGE('',*,*,#5096,.F.);
#6688=ORIENTED_EDGE('',*,*,#5091,.T.);
#6689=ORIENTED_EDGE('',*,*,#5092,.T.);
#6690=ORIENTED_EDGE('',*,*,#5106,.T.);
#6691=ORIENTED_EDGE('',*,*,#5099,.F.);
#6692=ORIENTED_EDGE('',*,*,#5106,.F.);
#6693=ORIENTED_EDGE('',*,*,#5107,.T.);
#6694=ORIENTED_EDGE('',*,*,#5107,.F.);
#6695=ORIENTED_EDGE('',*,*,#5108,.T.);
#6696=ORIENTED_EDGE('',*,*,#5108,.F.);
#6697=ORIENTED_EDGE('',*,*,#5109,.T.);
#6698=ORIENTED_EDGE('',*,*,#5109,.F.);
#6699=ORIENTED_EDGE('',*,*,#5110,.T.);
#6700=ORIENTED_EDGE('',*,*,#5110,.F.);
#6701=ORIENTED_EDGE('',*,*,#5111,.T.);
#6702=ORIENTED_EDGE('',*,*,#5111,.F.);
#6703=ORIENTED_EDGE('',*,*,#5112,.T.);
#6704=ORIENTED_EDGE('',*,*,#5112,.F.);
#6705=ORIENTED_EDGE('',*,*,#5113,.T.);
#6706=ORIENTED_EDGE('',*,*,#5113,.F.);
#6707=ORIENTED_EDGE('',*,*,#5114,.T.);
#6708=ORIENTED_EDGE('',*,*,#5114,.F.);
#6709=ORIENTED_EDGE('',*,*,#5115,.F.);
#6710=ORIENTED_EDGE('',*,*,#5116,.F.);
#6711=ORIENTED_EDGE('',*,*,#5117,.F.);
#6712=ORIENTED_EDGE('',*,*,#5118,.F.);
#6713=ORIENTED_EDGE('',*,*,#5117,.T.);
#6714=ORIENTED_EDGE('',*,*,#5119,.F.);
#6715=ORIENTED_EDGE('',*,*,#5120,.T.);
#6716=ORIENTED_EDGE('',*,*,#5121,.F.);
#6717=ORIENTED_EDGE('',*,*,#5122,.T.);
#6718=ORIENTED_EDGE('',*,*,#5123,.F.);
#6719=ORIENTED_EDGE('',*,*,#5124,.T.);
#6720=ORIENTED_EDGE('',*,*,#5125,.T.);
#6721=ORIENTED_EDGE('',*,*,#5126,.F.);
#6722=ORIENTED_EDGE('',*,*,#5125,.F.);
#6723=ORIENTED_EDGE('',*,*,#5127,.T.);
#6724=ORIENTED_EDGE('',*,*,#5128,.F.);
#6725=ORIENTED_EDGE('',*,*,#5129,.T.);
#6726=ORIENTED_EDGE('',*,*,#5130,.F.);
#6727=ORIENTED_EDGE('',*,*,#5131,.T.);
#6728=ORIENTED_EDGE('',*,*,#5132,.F.);
#6729=ORIENTED_EDGE('',*,*,#5133,.T.);
#6730=ORIENTED_EDGE('',*,*,#5134,.F.);
#6731=ORIENTED_EDGE('',*,*,#5135,.T.);
#6732=ORIENTED_EDGE('',*,*,#5136,.F.);
#6733=ORIENTED_EDGE('',*,*,#5116,.T.);
#6734=ORIENTED_EDGE('',*,*,#5137,.T.);
#6735=ORIENTED_EDGE('',*,*,#5138,.T.);
#6736=ORIENTED_EDGE('',*,*,#5119,.T.);
#6737=ORIENTED_EDGE('',*,*,#5139,.F.);
#6738=ORIENTED_EDGE('',*,*,#5140,.F.);
#6739=ORIENTED_EDGE('',*,*,#5120,.F.);
#6740=ORIENTED_EDGE('',*,*,#5138,.F.);
#6741=ORIENTED_EDGE('',*,*,#5140,.T.);
#6742=ORIENTED_EDGE('',*,*,#5141,.T.);
#6743=ORIENTED_EDGE('',*,*,#5142,.T.);
#6744=ORIENTED_EDGE('',*,*,#5121,.T.);
#6745=ORIENTED_EDGE('',*,*,#5143,.F.);
#6746=ORIENTED_EDGE('',*,*,#5144,.F.);
#6747=ORIENTED_EDGE('',*,*,#5122,.F.);
#6748=ORIENTED_EDGE('',*,*,#5142,.F.);
#6749=ORIENTED_EDGE('',*,*,#5144,.T.);
#6750=ORIENTED_EDGE('',*,*,#5145,.T.);
#6751=ORIENTED_EDGE('',*,*,#5146,.T.);
#6752=ORIENTED_EDGE('',*,*,#5123,.T.);
#6753=ORIENTED_EDGE('',*,*,#5147,.F.);
#6754=ORIENTED_EDGE('',*,*,#5148,.F.);
#6755=ORIENTED_EDGE('',*,*,#5127,.F.);
#6756=ORIENTED_EDGE('',*,*,#5124,.F.);
#6757=ORIENTED_EDGE('',*,*,#5146,.F.);
#6758=ORIENTED_EDGE('',*,*,#5149,.F.);
#6759=ORIENTED_EDGE('',*,*,#5148,.T.);
#6760=ORIENTED_EDGE('',*,*,#5150,.T.);
#6761=ORIENTED_EDGE('',*,*,#5151,.T.);
#6762=ORIENTED_EDGE('',*,*,#5128,.T.);
#6763=ORIENTED_EDGE('',*,*,#5152,.F.);
#6764=ORIENTED_EDGE('',*,*,#5153,.F.);
#6765=ORIENTED_EDGE('',*,*,#5129,.F.);
#6766=ORIENTED_EDGE('',*,*,#5151,.F.);
#6767=ORIENTED_EDGE('',*,*,#5153,.T.);
#6768=ORIENTED_EDGE('',*,*,#5154,.T.);
#6769=ORIENTED_EDGE('',*,*,#5155,.T.);
#6770=ORIENTED_EDGE('',*,*,#5130,.T.);
#6771=ORIENTED_EDGE('',*,*,#5156,.F.);
#6772=ORIENTED_EDGE('',*,*,#5157,.F.);
#6773=ORIENTED_EDGE('',*,*,#5131,.F.);
#6774=ORIENTED_EDGE('',*,*,#5155,.F.);
#6775=ORIENTED_EDGE('',*,*,#5157,.T.);
#6776=ORIENTED_EDGE('',*,*,#5158,.T.);
#6777=ORIENTED_EDGE('',*,*,#5159,.T.);
#6778=ORIENTED_EDGE('',*,*,#5132,.T.);
#6779=ORIENTED_EDGE('',*,*,#5133,.F.);
#6780=ORIENTED_EDGE('',*,*,#5159,.F.);
#6781=ORIENTED_EDGE('',*,*,#5160,.F.);
#6782=ORIENTED_EDGE('',*,*,#5161,.F.);
#6783=ORIENTED_EDGE('',*,*,#5162,.F.);
#6784=ORIENTED_EDGE('',*,*,#5163,.T.);
#6785=ORIENTED_EDGE('',*,*,#5149,.T.);
#6786=ORIENTED_EDGE('',*,*,#5145,.F.);
#6787=ORIENTED_EDGE('',*,*,#5143,.T.);
#6788=ORIENTED_EDGE('',*,*,#5141,.F.);
#6789=ORIENTED_EDGE('',*,*,#5139,.T.);
#6790=ORIENTED_EDGE('',*,*,#5137,.F.);
#6791=ORIENTED_EDGE('',*,*,#5115,.T.);
#6792=ORIENTED_EDGE('',*,*,#5164,.F.);
#6793=ORIENTED_EDGE('',*,*,#5165,.T.);
#6794=ORIENTED_EDGE('',*,*,#5166,.F.);
#6795=ORIENTED_EDGE('',*,*,#5160,.T.);
#6796=ORIENTED_EDGE('',*,*,#5158,.F.);
#6797=ORIENTED_EDGE('',*,*,#5156,.T.);
#6798=ORIENTED_EDGE('',*,*,#5154,.F.);
#6799=ORIENTED_EDGE('',*,*,#5152,.T.);
#6800=ORIENTED_EDGE('',*,*,#5150,.F.);
#6801=ORIENTED_EDGE('',*,*,#5147,.T.);
#6802=ORIENTED_EDGE('',*,*,#5163,.F.);
#6803=ORIENTED_EDGE('',*,*,#5118,.T.);
#6804=ORIENTED_EDGE('',*,*,#5136,.T.);
#6805=ORIENTED_EDGE('',*,*,#5167,.T.);
#6806=ORIENTED_EDGE('',*,*,#5164,.T.);
#6807=ORIENTED_EDGE('',*,*,#5135,.F.);
#6808=ORIENTED_EDGE('',*,*,#5168,.F.);
#6809=ORIENTED_EDGE('',*,*,#5165,.F.);
#6810=ORIENTED_EDGE('',*,*,#5167,.F.);
#6811=ORIENTED_EDGE('',*,*,#5126,.T.);
#6812=ORIENTED_EDGE('',*,*,#5162,.T.);
#6813=ORIENTED_EDGE('',*,*,#5161,.T.);
#6814=ORIENTED_EDGE('',*,*,#5166,.T.);
#6815=ORIENTED_EDGE('',*,*,#5168,.T.);
#6816=ORIENTED_EDGE('',*,*,#5134,.T.);
#6817=ORIENTED_EDGE('',*,*,#5169,.F.);
#6818=ORIENTED_EDGE('',*,*,#5170,.T.);
#6819=ORIENTED_EDGE('',*,*,#5171,.F.);
#6820=ORIENTED_EDGE('',*,*,#5172,.T.);
#6821=ORIENTED_EDGE('',*,*,#5169,.T.);
#6822=ORIENTED_EDGE('',*,*,#5172,.F.);
#6823=ORIENTED_EDGE('',*,*,#5171,.T.);
#6824=ORIENTED_EDGE('',*,*,#5173,.F.);
#6825=ORIENTED_EDGE('',*,*,#5173,.T.);
#6826=ORIENTED_EDGE('',*,*,#5174,.T.);
#6827=ORIENTED_EDGE('',*,*,#5170,.F.);
#6828=ORIENTED_EDGE('',*,*,#5174,.F.);
#6829=ORIENTED_EDGE('',*,*,#5175,.F.);
#6830=ORIENTED_EDGE('',*,*,#5176,.T.);
#6831=ORIENTED_EDGE('',*,*,#5177,.F.);
#6832=ORIENTED_EDGE('',*,*,#5178,.T.);
#6833=ORIENTED_EDGE('',*,*,#5175,.T.);
#6834=ORIENTED_EDGE('',*,*,#5178,.F.);
#6835=ORIENTED_EDGE('',*,*,#5177,.T.);
#6836=ORIENTED_EDGE('',*,*,#5179,.F.);
#6837=ORIENTED_EDGE('',*,*,#5179,.T.);
#6838=ORIENTED_EDGE('',*,*,#5180,.T.);
#6839=ORIENTED_EDGE('',*,*,#5176,.F.);
#6840=ORIENTED_EDGE('',*,*,#5180,.F.);
#6841=ORIENTED_EDGE('',*,*,#5181,.F.);
#6842=ORIENTED_EDGE('',*,*,#5182,.F.);
#6843=ORIENTED_EDGE('',*,*,#5183,.F.);
#6844=ORIENTED_EDGE('',*,*,#5184,.F.);
#6845=ORIENTED_EDGE('',*,*,#5185,.F.);
#6846=ORIENTED_EDGE('',*,*,#5184,.T.);
#6847=ORIENTED_EDGE('',*,*,#5186,.F.);
#6848=ORIENTED_EDGE('',*,*,#5187,.T.);
#6849=ORIENTED_EDGE('',*,*,#5188,.F.);
#6850=ORIENTED_EDGE('',*,*,#5187,.F.);
#6851=ORIENTED_EDGE('',*,*,#5189,.F.);
#6852=ORIENTED_EDGE('',*,*,#5190,.F.);
#6853=ORIENTED_EDGE('',*,*,#5191,.F.);
#6854=ORIENTED_EDGE('',*,*,#5190,.T.);
#6855=ORIENTED_EDGE('',*,*,#5192,.T.);
#6856=ORIENTED_EDGE('',*,*,#5182,.T.);
#6857=ORIENTED_EDGE('',*,*,#5192,.F.);
#6858=ORIENTED_EDGE('',*,*,#5189,.T.);
#6859=ORIENTED_EDGE('',*,*,#5186,.T.);
#6860=ORIENTED_EDGE('',*,*,#5183,.T.);
#6861=ORIENTED_EDGE('',*,*,#5193,.F.);
#6862=ORIENTED_EDGE('',*,*,#5194,.T.);
#6863=ORIENTED_EDGE('',*,*,#5195,.F.);
#6864=ORIENTED_EDGE('',*,*,#5196,.T.);
#6865=ORIENTED_EDGE('',*,*,#5193,.T.);
#6866=ORIENTED_EDGE('',*,*,#5196,.F.);
#6867=ORIENTED_EDGE('',*,*,#5195,.T.);
#6868=ORIENTED_EDGE('',*,*,#5197,.F.);
#6869=ORIENTED_EDGE('',*,*,#5198,.F.);
#6870=ORIENTED_EDGE('',*,*,#5199,.T.);
#6871=ORIENTED_EDGE('',*,*,#5197,.T.);
#6872=ORIENTED_EDGE('',*,*,#5199,.F.);
#6873=ORIENTED_EDGE('',*,*,#5200,.F.);
#6874=ORIENTED_EDGE('',*,*,#5198,.T.);
#6875=ORIENTED_EDGE('',*,*,#5201,.F.);
#6876=ORIENTED_EDGE('',*,*,#5202,.T.);
#6877=ORIENTED_EDGE('',*,*,#5200,.T.);
#6878=ORIENTED_EDGE('',*,*,#5202,.F.);
#6879=ORIENTED_EDGE('',*,*,#5201,.T.);
#6880=ORIENTED_EDGE('',*,*,#5203,.F.);
#6881=ORIENTED_EDGE('',*,*,#5204,.F.);
#6882=ORIENTED_EDGE('',*,*,#5205,.T.);
#6883=ORIENTED_EDGE('',*,*,#5203,.T.);
#6884=ORIENTED_EDGE('',*,*,#5205,.F.);
#6885=ORIENTED_EDGE('',*,*,#5206,.F.);
#6886=ORIENTED_EDGE('',*,*,#5204,.T.);
#6887=ORIENTED_EDGE('',*,*,#5207,.F.);
#6888=ORIENTED_EDGE('',*,*,#5208,.T.);
#6889=ORIENTED_EDGE('',*,*,#5206,.T.);
#6890=ORIENTED_EDGE('',*,*,#5208,.F.);
#6891=ORIENTED_EDGE('',*,*,#5207,.T.);
#6892=ORIENTED_EDGE('',*,*,#5209,.F.);
#6893=ORIENTED_EDGE('',*,*,#5209,.T.);
#6894=ORIENTED_EDGE('',*,*,#5210,.T.);
#6895=ORIENTED_EDGE('',*,*,#5194,.F.);
#6896=ORIENTED_EDGE('',*,*,#5210,.F.);
#6897=ORIENTED_EDGE('',*,*,#5188,.T.);
#6898=ORIENTED_EDGE('',*,*,#5191,.T.);
#6899=ORIENTED_EDGE('',*,*,#5181,.T.);
#6900=ORIENTED_EDGE('',*,*,#5185,.T.);
#6901=ORIENTED_EDGE('',*,*,#5211,.F.);
#6902=ORIENTED_EDGE('',*,*,#5212,.F.);
#6903=ORIENTED_EDGE('',*,*,#5213,.F.);
#6904=ORIENTED_EDGE('',*,*,#5214,.F.);
#6905=ORIENTED_EDGE('',*,*,#5215,.F.);
#6906=ORIENTED_EDGE('',*,*,#5214,.T.);
#6907=ORIENTED_EDGE('',*,*,#5216,.F.);
#6908=ORIENTED_EDGE('',*,*,#5217,.T.);
#6909=ORIENTED_EDGE('',*,*,#5218,.F.);
#6910=ORIENTED_EDGE('',*,*,#5217,.F.);
#6911=ORIENTED_EDGE('',*,*,#5219,.F.);
#6912=ORIENTED_EDGE('',*,*,#5220,.F.);
#6913=ORIENTED_EDGE('',*,*,#5221,.F.);
#6914=ORIENTED_EDGE('',*,*,#5220,.T.);
#6915=ORIENTED_EDGE('',*,*,#5222,.F.);
#6916=ORIENTED_EDGE('',*,*,#5212,.T.);
#6917=ORIENTED_EDGE('',*,*,#5223,.F.);
#6918=ORIENTED_EDGE('',*,*,#5224,.T.);
#6919=ORIENTED_EDGE('',*,*,#5225,.F.);
#6920=ORIENTED_EDGE('',*,*,#5226,.T.);
#6921=ORIENTED_EDGE('',*,*,#5223,.T.);
#6922=ORIENTED_EDGE('',*,*,#5226,.F.);
#6923=ORIENTED_EDGE('',*,*,#5218,.T.);
#6924=ORIENTED_EDGE('',*,*,#5221,.T.);
#6925=ORIENTED_EDGE('',*,*,#5211,.T.);
#6926=ORIENTED_EDGE('',*,*,#5215,.T.);
#6927=ORIENTED_EDGE('',*,*,#5225,.T.);
#6928=ORIENTED_EDGE('',*,*,#5227,.F.);
#6929=ORIENTED_EDGE('',*,*,#5227,.T.);
#6930=ORIENTED_EDGE('',*,*,#5228,.T.);
#6931=ORIENTED_EDGE('',*,*,#5224,.F.);
#6932=ORIENTED_EDGE('',*,*,#5228,.F.);
#6933=ORIENTED_EDGE('',*,*,#5219,.T.);
#6934=ORIENTED_EDGE('',*,*,#5216,.T.);
#6935=ORIENTED_EDGE('',*,*,#5213,.T.);
#6936=ORIENTED_EDGE('',*,*,#5222,.T.);
#6937=ORIENTED_EDGE('',*,*,#5229,.T.);
#6938=ORIENTED_EDGE('',*,*,#5230,.T.);
#6939=ORIENTED_EDGE('',*,*,#5231,.T.);
#6940=ORIENTED_EDGE('',*,*,#5232,.F.);
#6941=ORIENTED_EDGE('',*,*,#5233,.T.);
#6942=ORIENTED_EDGE('',*,*,#5234,.T.);
#6943=ORIENTED_EDGE('',*,*,#5235,.T.);
#6944=ORIENTED_EDGE('',*,*,#5230,.F.);
#6945=ORIENTED_EDGE('',*,*,#5236,.T.);
#6946=ORIENTED_EDGE('',*,*,#5237,.T.);
#6947=ORIENTED_EDGE('',*,*,#5238,.T.);
#6948=ORIENTED_EDGE('',*,*,#5234,.F.);
#6949=ORIENTED_EDGE('',*,*,#5239,.T.);
#6950=ORIENTED_EDGE('',*,*,#5240,.T.);
#6951=ORIENTED_EDGE('',*,*,#5241,.T.);
#6952=ORIENTED_EDGE('',*,*,#5237,.F.);
#6953=ORIENTED_EDGE('',*,*,#5242,.T.);
#6954=ORIENTED_EDGE('',*,*,#5243,.T.);
#6955=ORIENTED_EDGE('',*,*,#5244,.T.);
#6956=ORIENTED_EDGE('',*,*,#5240,.F.);
#6957=ORIENTED_EDGE('',*,*,#5245,.T.);
#6958=ORIENTED_EDGE('',*,*,#5232,.T.);
#6959=ORIENTED_EDGE('',*,*,#5246,.T.);
#6960=ORIENTED_EDGE('',*,*,#5243,.F.);
#6961=ORIENTED_EDGE('',*,*,#5245,.F.);
#6962=ORIENTED_EDGE('',*,*,#5242,.F.);
#6963=ORIENTED_EDGE('',*,*,#5239,.F.);
#6964=ORIENTED_EDGE('',*,*,#5236,.F.);
#6965=ORIENTED_EDGE('',*,*,#5233,.F.);
#6966=ORIENTED_EDGE('',*,*,#5229,.F.);
#6967=ORIENTED_EDGE('',*,*,#5246,.F.);
#6968=ORIENTED_EDGE('',*,*,#5231,.F.);
#6969=ORIENTED_EDGE('',*,*,#5235,.F.);
#6970=ORIENTED_EDGE('',*,*,#5238,.F.);
#6971=ORIENTED_EDGE('',*,*,#5241,.F.);
#6972=ORIENTED_EDGE('',*,*,#5244,.F.);
#6973=ORIENTED_EDGE('',*,*,#5247,.T.);
#6974=ORIENTED_EDGE('',*,*,#5248,.T.);
#6975=ORIENTED_EDGE('',*,*,#5247,.F.);
#6976=ORIENTED_EDGE('',*,*,#5249,.T.);
#6977=ORIENTED_EDGE('',*,*,#5250,.T.);
#6978=ORIENTED_EDGE('',*,*,#5249,.F.);
#6979=ORIENTED_EDGE('',*,*,#5250,.F.);
#6980=ORIENTED_EDGE('',*,*,#5251,.F.);
#6981=ORIENTED_EDGE('',*,*,#5252,.F.);
#6982=ORIENTED_EDGE('',*,*,#5253,.T.);
#6983=ORIENTED_EDGE('',*,*,#5251,.T.);
#6984=ORIENTED_EDGE('',*,*,#5253,.F.);
#6985=ORIENTED_EDGE('',*,*,#5254,.F.);
#6986=ORIENTED_EDGE('',*,*,#5255,.T.);
#6987=ORIENTED_EDGE('',*,*,#5252,.T.);
#6988=ORIENTED_EDGE('',*,*,#5255,.F.);
#6989=ORIENTED_EDGE('',*,*,#5256,.F.);
#6990=ORIENTED_EDGE('',*,*,#5257,.T.);
#6991=ORIENTED_EDGE('',*,*,#5254,.T.);
#6992=ORIENTED_EDGE('',*,*,#5257,.F.);
#6993=ORIENTED_EDGE('',*,*,#5256,.T.);
#6994=ORIENTED_EDGE('',*,*,#5258,.F.);
#6995=ORIENTED_EDGE('',*,*,#5259,.F.);
#6996=ORIENTED_EDGE('',*,*,#5260,.T.);
#6997=ORIENTED_EDGE('',*,*,#5258,.T.);
#6998=ORIENTED_EDGE('',*,*,#5260,.F.);
#6999=ORIENTED_EDGE('',*,*,#5261,.F.);
#7000=ORIENTED_EDGE('',*,*,#5262,.T.);
#7001=ORIENTED_EDGE('',*,*,#5259,.T.);
#7002=ORIENTED_EDGE('',*,*,#5262,.F.);
#7003=ORIENTED_EDGE('',*,*,#5248,.F.);
#7004=ORIENTED_EDGE('',*,*,#5263,.T.);
#7005=ORIENTED_EDGE('',*,*,#5261,.T.);
#7006=ORIENTED_EDGE('',*,*,#5263,.F.);
#7007=ORIENTED_EDGE('',*,*,#5264,.F.);
#7008=ORIENTED_EDGE('',*,*,#5265,.T.);
#7009=ORIENTED_EDGE('',*,*,#5266,.F.);
#7010=ORIENTED_EDGE('',*,*,#5265,.F.);
#7011=ORIENTED_EDGE('',*,*,#5267,.F.);
#7012=ORIENTED_EDGE('',*,*,#5268,.F.);
#7013=ORIENTED_EDGE('',*,*,#5269,.F.);
#7014=ORIENTED_EDGE('',*,*,#5270,.T.);
#7015=ORIENTED_EDGE('',*,*,#5270,.F.);
#7016=ORIENTED_EDGE('',*,*,#5271,.F.);
#7017=ORIENTED_EDGE('',*,*,#5272,.F.);
#7018=ORIENTED_EDGE('',*,*,#5273,.F.);
#7019=ORIENTED_EDGE('',*,*,#5274,.F.);
#7020=ORIENTED_EDGE('',*,*,#5275,.F.);
#7021=ORIENTED_EDGE('',*,*,#5276,.F.);
#7022=ORIENTED_EDGE('',*,*,#5277,.F.);
#7023=ORIENTED_EDGE('',*,*,#5278,.F.);
#7024=ORIENTED_EDGE('',*,*,#5264,.T.);
#7025=ORIENTED_EDGE('',*,*,#5279,.F.);
#7026=ORIENTED_EDGE('',*,*,#5269,.T.);
#7027=ORIENTED_EDGE('',*,*,#5280,.F.);
#7028=ORIENTED_EDGE('',*,*,#5281,.F.);
#7029=ORIENTED_EDGE('',*,*,#5271,.T.);
#7030=ORIENTED_EDGE('',*,*,#5282,.T.);
#7031=ORIENTED_EDGE('',*,*,#5283,.F.);
#7032=ORIENTED_EDGE('',*,*,#5280,.T.);
#7033=ORIENTED_EDGE('',*,*,#5268,.T.);
#7034=ORIENTED_EDGE('',*,*,#5267,.T.);
#7035=ORIENTED_EDGE('',*,*,#5278,.T.);
#7036=ORIENTED_EDGE('',*,*,#5284,.F.);
#7037=ORIENTED_EDGE('',*,*,#5282,.F.);
#7038=ORIENTED_EDGE('',*,*,#5285,.F.);
#7039=ORIENTED_EDGE('',*,*,#5286,.F.);
#7040=ORIENTED_EDGE('',*,*,#5287,.F.);
#7041=ORIENTED_EDGE('',*,*,#5275,.T.);
#7042=ORIENTED_EDGE('',*,*,#5287,.T.);
#7043=ORIENTED_EDGE('',*,*,#5288,.F.);
#7044=ORIENTED_EDGE('',*,*,#5289,.F.);
#7045=ORIENTED_EDGE('',*,*,#5276,.T.);
#7046=ORIENTED_EDGE('',*,*,#5290,.T.);
#7047=ORIENTED_EDGE('',*,*,#5291,.F.);
#7048=ORIENTED_EDGE('',*,*,#5288,.T.);
#7049=ORIENTED_EDGE('',*,*,#5286,.T.);
#7050=ORIENTED_EDGE('',*,*,#5266,.T.);
#7051=ORIENTED_EDGE('',*,*,#5285,.T.);
#7052=ORIENTED_EDGE('',*,*,#5274,.T.);
#7053=ORIENTED_EDGE('',*,*,#5292,.F.);
#7054=ORIENTED_EDGE('',*,*,#5290,.F.);
#7055=ORIENTED_EDGE('',*,*,#5293,.T.);
#7056=ORIENTED_EDGE('',*,*,#5294,.F.);
#7057=ORIENTED_EDGE('',*,*,#5293,.F.);
#7058=ORIENTED_EDGE('',*,*,#5295,.T.);
#7059=ORIENTED_EDGE('',*,*,#5272,.T.);
#7060=ORIENTED_EDGE('',*,*,#5281,.T.);
#7061=ORIENTED_EDGE('',*,*,#5283,.T.);
#7062=ORIENTED_EDGE('',*,*,#5284,.T.);
#7063=ORIENTED_EDGE('',*,*,#5277,.T.);
#7064=ORIENTED_EDGE('',*,*,#5289,.T.);
#7065=ORIENTED_EDGE('',*,*,#5291,.T.);
#7066=ORIENTED_EDGE('',*,*,#5292,.T.);
#7067=ORIENTED_EDGE('',*,*,#5273,.T.);
#7068=ORIENTED_EDGE('',*,*,#5295,.F.);
#7069=ORIENTED_EDGE('',*,*,#5296,.T.);
#7070=ORIENTED_EDGE('',*,*,#5297,.F.);
#7071=ORIENTED_EDGE('',*,*,#5296,.F.);
#7072=ORIENTED_EDGE('',*,*,#5298,.T.);
#7073=ORIENTED_EDGE('',*,*,#5294,.T.);
#7074=ORIENTED_EDGE('',*,*,#5298,.F.);
#7075=ORIENTED_EDGE('',*,*,#5279,.T.);
#7076=ORIENTED_EDGE('',*,*,#5299,.T.);
#7077=ORIENTED_EDGE('',*,*,#5300,.T.);
#7078=ORIENTED_EDGE('',*,*,#5299,.F.);
#7079=ORIENTED_EDGE('',*,*,#5301,.F.);
#7080=ORIENTED_EDGE('',*,*,#5302,.T.);
#7081=ORIENTED_EDGE('',*,*,#5297,.T.);
#7082=ORIENTED_EDGE('',*,*,#5302,.F.);
#7083=ORIENTED_EDGE('',*,*,#5301,.T.);
#7084=ORIENTED_EDGE('',*,*,#5300,.F.);
#7085=ORIENTED_EDGE('',*,*,#5303,.F.);
#7086=ORIENTED_EDGE('',*,*,#5304,.T.);
#7087=ORIENTED_EDGE('',*,*,#5305,.T.);
#7088=ORIENTED_EDGE('',*,*,#5304,.F.);
#7089=ORIENTED_EDGE('',*,*,#5306,.F.);
#7090=ORIENTED_EDGE('',*,*,#5307,.T.);
#7091=ORIENTED_EDGE('',*,*,#5308,.T.);
#7092=ORIENTED_EDGE('',*,*,#5307,.F.);
#7093=ORIENTED_EDGE('',*,*,#5306,.T.);
#7094=ORIENTED_EDGE('',*,*,#5303,.T.);
#7095=ORIENTED_EDGE('',*,*,#5308,.F.);
#7096=ORIENTED_EDGE('',*,*,#5305,.F.);
#7097=ORIENTED_EDGE('',*,*,#5309,.F.);
#7098=ORIENTED_EDGE('',*,*,#5310,.T.);
#7099=ORIENTED_EDGE('',*,*,#5311,.F.);
#7100=ORIENTED_EDGE('',*,*,#5312,.F.);
#7101=ORIENTED_EDGE('',*,*,#5313,.T.);
#7102=ORIENTED_EDGE('',*,*,#5314,.F.);
#7103=ORIENTED_EDGE('',*,*,#5315,.F.);
#7104=ORIENTED_EDGE('',*,*,#5313,.F.);
#7105=ORIENTED_EDGE('',*,*,#5316,.F.);
#7106=ORIENTED_EDGE('',*,*,#5317,.F.);
#7107=ORIENTED_EDGE('',*,*,#5310,.F.);
#7108=ORIENTED_EDGE('',*,*,#5318,.F.);
#7109=ORIENTED_EDGE('',*,*,#5316,.T.);
#7110=ORIENTED_EDGE('',*,*,#5312,.T.);
#7111=ORIENTED_EDGE('',*,*,#5319,.F.);
#7112=ORIENTED_EDGE('',*,*,#5320,.T.);
#7113=ORIENTED_EDGE('',*,*,#5321,.T.);
#7114=ORIENTED_EDGE('',*,*,#5320,.F.);
#7115=ORIENTED_EDGE('',*,*,#5317,.T.);
#7116=ORIENTED_EDGE('',*,*,#5318,.T.);
#7117=ORIENTED_EDGE('',*,*,#5311,.T.);
#7118=ORIENTED_EDGE('',*,*,#5309,.T.);
#7119=ORIENTED_EDGE('',*,*,#5322,.F.);
#7120=ORIENTED_EDGE('',*,*,#5323,.T.);
#7121=ORIENTED_EDGE('',*,*,#5324,.T.);
#7122=ORIENTED_EDGE('',*,*,#5323,.F.);
#7123=ORIENTED_EDGE('',*,*,#5314,.T.);
#7124=ORIENTED_EDGE('',*,*,#5315,.T.);
#7125=ORIENTED_EDGE('',*,*,#5322,.T.);
#7126=ORIENTED_EDGE('',*,*,#5319,.T.);
#7127=ORIENTED_EDGE('',*,*,#5324,.F.);
#7128=ORIENTED_EDGE('',*,*,#5321,.F.);
#7129=ORIENTED_EDGE('',*,*,#5325,.F.);
#7130=ORIENTED_EDGE('',*,*,#5326,.T.);
#7131=ORIENTED_EDGE('',*,*,#5327,.F.);
#7132=ORIENTED_EDGE('',*,*,#5326,.F.);
#7133=ORIENTED_EDGE('',*,*,#5325,.T.);
#7134=ORIENTED_EDGE('',*,*,#5328,.F.);
#7135=ORIENTED_EDGE('',*,*,#5329,.T.);
#7136=ORIENTED_EDGE('',*,*,#5330,.T.);
#7137=ORIENTED_EDGE('',*,*,#5329,.F.);
#7138=ORIENTED_EDGE('',*,*,#5330,.F.);
#7139=ORIENTED_EDGE('',*,*,#5331,.T.);
#7140=ORIENTED_EDGE('',*,*,#5332,.F.);
#7141=ORIENTED_EDGE('',*,*,#5333,.F.);
#7142=ORIENTED_EDGE('',*,*,#5334,.F.);
#7143=ORIENTED_EDGE('',*,*,#5331,.F.);
#7144=ORIENTED_EDGE('',*,*,#5335,.T.);
#7145=ORIENTED_EDGE('',*,*,#5333,.T.);
#7146=ORIENTED_EDGE('',*,*,#5335,.F.);
#7147=ORIENTED_EDGE('',*,*,#5334,.T.);
#7148=ORIENTED_EDGE('',*,*,#5336,.T.);
#7149=ORIENTED_EDGE('',*,*,#5337,.T.);
#7150=ORIENTED_EDGE('',*,*,#5336,.F.);
#7151=ORIENTED_EDGE('',*,*,#5338,.F.);
#7152=ORIENTED_EDGE('',*,*,#5339,.T.);
#7153=ORIENTED_EDGE('',*,*,#5332,.T.);
#7154=ORIENTED_EDGE('',*,*,#5339,.F.);
#7155=ORIENTED_EDGE('',*,*,#5338,.T.);
#7156=ORIENTED_EDGE('',*,*,#5327,.T.);
#7157=ORIENTED_EDGE('',*,*,#5337,.F.);
#7158=ORIENTED_EDGE('',*,*,#5328,.T.);
#7159=ORIENTED_EDGE('',*,*,#5340,.F.);
#7160=ORIENTED_EDGE('',*,*,#5341,.T.);
#7161=ORIENTED_EDGE('',*,*,#5342,.T.);
#7162=ORIENTED_EDGE('',*,*,#5341,.F.);
#7163=ORIENTED_EDGE('',*,*,#5343,.F.);
#7164=ORIENTED_EDGE('',*,*,#5344,.T.);
#7165=ORIENTED_EDGE('',*,*,#5345,.T.);
#7166=ORIENTED_EDGE('',*,*,#5344,.F.);
#7167=ORIENTED_EDGE('',*,*,#5343,.T.);
#7168=ORIENTED_EDGE('',*,*,#5340,.T.);
#7169=ORIENTED_EDGE('',*,*,#5345,.F.);
#7170=ORIENTED_EDGE('',*,*,#5342,.F.);
#7171=ORIENTED_EDGE('',*,*,#5346,.F.);
#7172=ORIENTED_EDGE('',*,*,#5347,.T.);
#7173=ORIENTED_EDGE('',*,*,#5348,.T.);
#7174=ORIENTED_EDGE('',*,*,#5347,.F.);
#7175=ORIENTED_EDGE('',*,*,#5349,.F.);
#7176=ORIENTED_EDGE('',*,*,#5350,.T.);
#7177=ORIENTED_EDGE('',*,*,#5351,.T.);
#7178=ORIENTED_EDGE('',*,*,#5350,.F.);
#7179=ORIENTED_EDGE('',*,*,#5349,.T.);
#7180=ORIENTED_EDGE('',*,*,#5346,.T.);
#7181=ORIENTED_EDGE('',*,*,#5351,.F.);
#7182=ORIENTED_EDGE('',*,*,#5348,.F.);
#7183=ORIENTED_EDGE('',*,*,#5352,.F.);
#7184=ORIENTED_EDGE('',*,*,#5353,.T.);
#7185=ORIENTED_EDGE('',*,*,#5354,.T.);
#7186=ORIENTED_EDGE('',*,*,#5353,.F.);
#7187=ORIENTED_EDGE('',*,*,#5355,.F.);
#7188=ORIENTED_EDGE('',*,*,#5356,.T.);
#7189=ORIENTED_EDGE('',*,*,#5357,.T.);
#7190=ORIENTED_EDGE('',*,*,#5356,.F.);
#7191=ORIENTED_EDGE('',*,*,#5355,.T.);
#7192=ORIENTED_EDGE('',*,*,#5352,.T.);
#7193=ORIENTED_EDGE('',*,*,#5357,.F.);
#7194=ORIENTED_EDGE('',*,*,#5354,.F.);
#7195=ORIENTED_EDGE('',*,*,#5358,.F.);
#7196=ORIENTED_EDGE('',*,*,#5359,.T.);
#7197=ORIENTED_EDGE('',*,*,#5360,.T.);
#7198=ORIENTED_EDGE('',*,*,#5359,.F.);
#7199=ORIENTED_EDGE('',*,*,#5361,.F.);
#7200=ORIENTED_EDGE('',*,*,#5362,.T.);
#7201=ORIENTED_EDGE('',*,*,#5363,.T.);
#7202=ORIENTED_EDGE('',*,*,#5362,.F.);
#7203=ORIENTED_EDGE('',*,*,#5361,.T.);
#7204=ORIENTED_EDGE('',*,*,#5358,.T.);
#7205=ORIENTED_EDGE('',*,*,#5363,.F.);
#7206=ORIENTED_EDGE('',*,*,#5360,.F.);
#7207=ORIENTED_EDGE('',*,*,#5364,.F.);
#7208=ORIENTED_EDGE('',*,*,#5365,.F.);
#7209=ORIENTED_EDGE('',*,*,#5366,.T.);
#7210=ORIENTED_EDGE('',*,*,#5367,.T.);
#7211=ORIENTED_EDGE('',*,*,#5368,.F.);
#7212=ORIENTED_EDGE('',*,*,#5369,.F.);
#7213=ORIENTED_EDGE('',*,*,#5370,.T.);
#7214=ORIENTED_EDGE('',*,*,#5371,.T.);
#7215=ORIENTED_EDGE('',*,*,#5366,.F.);
#7216=ORIENTED_EDGE('',*,*,#5372,.F.);
#7217=ORIENTED_EDGE('',*,*,#5373,.T.);
#7218=ORIENTED_EDGE('',*,*,#5374,.T.);
#7219=ORIENTED_EDGE('',*,*,#5370,.F.);
#7220=ORIENTED_EDGE('',*,*,#5375,.F.);
#7221=ORIENTED_EDGE('',*,*,#5376,.T.);
#7222=ORIENTED_EDGE('',*,*,#5377,.T.);
#7223=ORIENTED_EDGE('',*,*,#5373,.F.);
#7224=ORIENTED_EDGE('',*,*,#5378,.F.);
#7225=ORIENTED_EDGE('',*,*,#5379,.T.);
#7226=ORIENTED_EDGE('',*,*,#5380,.T.);
#7227=ORIENTED_EDGE('',*,*,#5376,.F.);
#7228=ORIENTED_EDGE('',*,*,#5381,.F.);
#7229=ORIENTED_EDGE('',*,*,#5368,.T.);
#7230=ORIENTED_EDGE('',*,*,#5382,.T.);
#7231=ORIENTED_EDGE('',*,*,#5379,.F.);
#7232=ORIENTED_EDGE('',*,*,#5382,.F.);
#7233=ORIENTED_EDGE('',*,*,#5367,.F.);
#7234=ORIENTED_EDGE('',*,*,#5371,.F.);
#7235=ORIENTED_EDGE('',*,*,#5374,.F.);
#7236=ORIENTED_EDGE('',*,*,#5377,.F.);
#7237=ORIENTED_EDGE('',*,*,#5380,.F.);
#7238=ORIENTED_EDGE('',*,*,#5383,.F.);
#7239=ORIENTED_EDGE('',*,*,#5365,.T.);
#7240=ORIENTED_EDGE('',*,*,#5381,.T.);
#7241=ORIENTED_EDGE('',*,*,#5378,.T.);
#7242=ORIENTED_EDGE('',*,*,#5375,.T.);
#7243=ORIENTED_EDGE('',*,*,#5372,.T.);
#7244=ORIENTED_EDGE('',*,*,#5369,.T.);
#7245=ORIENTED_EDGE('',*,*,#5384,.F.);
#7246=ORIENTED_EDGE('',*,*,#5385,.T.);
#7247=ORIENTED_EDGE('',*,*,#5383,.T.);
#7248=ORIENTED_EDGE('',*,*,#5385,.F.);
#7249=ORIENTED_EDGE('',*,*,#5364,.T.);
#7250=ORIENTED_EDGE('',*,*,#5386,.T.);
#7251=ORIENTED_EDGE('',*,*,#5384,.T.);
#7252=ORIENTED_EDGE('',*,*,#5386,.F.);
#7253=ORIENTED_EDGE('',*,*,#5387,.T.);
#7254=ORIENTED_EDGE('',*,*,#5388,.T.);
#7255=ORIENTED_EDGE('',*,*,#5389,.T.);
#7256=ORIENTED_EDGE('',*,*,#5390,.F.);
#7257=ORIENTED_EDGE('',*,*,#5391,.T.);
#7258=ORIENTED_EDGE('',*,*,#5392,.T.);
#7259=ORIENTED_EDGE('',*,*,#5393,.T.);
#7260=ORIENTED_EDGE('',*,*,#5388,.F.);
#7261=ORIENTED_EDGE('',*,*,#5394,.T.);
#7262=ORIENTED_EDGE('',*,*,#5395,.T.);
#7263=ORIENTED_EDGE('',*,*,#5396,.T.);
#7264=ORIENTED_EDGE('',*,*,#5392,.F.);
#7265=ORIENTED_EDGE('',*,*,#5397,.T.);
#7266=ORIENTED_EDGE('',*,*,#5398,.T.);
#7267=ORIENTED_EDGE('',*,*,#5399,.T.);
#7268=ORIENTED_EDGE('',*,*,#5395,.F.);
#7269=ORIENTED_EDGE('',*,*,#5400,.T.);
#7270=ORIENTED_EDGE('',*,*,#5401,.T.);
#7271=ORIENTED_EDGE('',*,*,#5402,.T.);
#7272=ORIENTED_EDGE('',*,*,#5398,.F.);
#7273=ORIENTED_EDGE('',*,*,#5403,.T.);
#7274=ORIENTED_EDGE('',*,*,#5390,.T.);
#7275=ORIENTED_EDGE('',*,*,#5404,.T.);
#7276=ORIENTED_EDGE('',*,*,#5401,.F.);
#7277=ORIENTED_EDGE('',*,*,#5403,.F.);
#7278=ORIENTED_EDGE('',*,*,#5400,.F.);
#7279=ORIENTED_EDGE('',*,*,#5397,.F.);
#7280=ORIENTED_EDGE('',*,*,#5394,.F.);
#7281=ORIENTED_EDGE('',*,*,#5391,.F.);
#7282=ORIENTED_EDGE('',*,*,#5387,.F.);
#7283=ORIENTED_EDGE('',*,*,#5404,.F.);
#7284=ORIENTED_EDGE('',*,*,#5389,.F.);
#7285=ORIENTED_EDGE('',*,*,#5393,.F.);
#7286=ORIENTED_EDGE('',*,*,#5396,.F.);
#7287=ORIENTED_EDGE('',*,*,#5399,.F.);
#7288=ORIENTED_EDGE('',*,*,#5402,.F.);
#7289=ORIENTED_EDGE('',*,*,#5405,.F.);
#7290=ORIENTED_EDGE('',*,*,#5406,.F.);
#7291=ORIENTED_EDGE('',*,*,#5407,.F.);
#7292=ORIENTED_EDGE('',*,*,#5408,.T.);
#7293=ORIENTED_EDGE('',*,*,#5406,.T.);
#7294=ORIENTED_EDGE('',*,*,#5408,.F.);
#7295=ORIENTED_EDGE('',*,*,#5409,.F.);
#7296=ORIENTED_EDGE('',*,*,#5410,.T.);
#7297=ORIENTED_EDGE('',*,*,#5407,.T.);
#7298=ORIENTED_EDGE('',*,*,#5410,.F.);
#7299=ORIENTED_EDGE('',*,*,#5411,.F.);
#7300=ORIENTED_EDGE('',*,*,#5412,.T.);
#7301=ORIENTED_EDGE('',*,*,#5409,.T.);
#7302=ORIENTED_EDGE('',*,*,#5412,.F.);
#7303=ORIENTED_EDGE('',*,*,#5411,.T.);
#7304=ORIENTED_EDGE('',*,*,#5413,.F.);
#7305=ORIENTED_EDGE('',*,*,#5414,.F.);
#7306=ORIENTED_EDGE('',*,*,#5415,.T.);
#7307=ORIENTED_EDGE('',*,*,#5413,.T.);
#7308=ORIENTED_EDGE('',*,*,#5415,.F.);
#7309=ORIENTED_EDGE('',*,*,#5405,.T.);
#7310=ORIENTED_EDGE('',*,*,#5416,.T.);
#7311=ORIENTED_EDGE('',*,*,#5414,.T.);
#7312=ORIENTED_EDGE('',*,*,#5416,.F.);
#7313=ORIENTED_EDGE('',*,*,#5417,.F.);
#7314=ORIENTED_EDGE('',*,*,#5418,.F.);
#7315=ORIENTED_EDGE('',*,*,#5419,.T.);
#7316=ORIENTED_EDGE('',*,*,#5417,.T.);
#7317=ORIENTED_EDGE('',*,*,#5419,.F.);
#7318=ORIENTED_EDGE('',*,*,#5420,.F.);
#7319=ORIENTED_EDGE('',*,*,#5421,.T.);
#7320=ORIENTED_EDGE('',*,*,#5418,.T.);
#7321=ORIENTED_EDGE('',*,*,#5421,.F.);
#7322=ORIENTED_EDGE('',*,*,#5422,.F.);
#7323=ORIENTED_EDGE('',*,*,#5423,.T.);
#7324=ORIENTED_EDGE('',*,*,#5420,.T.);
#7325=ORIENTED_EDGE('',*,*,#5423,.F.);
#7326=ORIENTED_EDGE('',*,*,#5422,.T.);
#7327=ORIENTED_EDGE('',*,*,#5424,.F.);
#7328=ORIENTED_EDGE('',*,*,#5425,.F.);
#7329=ORIENTED_EDGE('',*,*,#5426,.T.);
#7330=ORIENTED_EDGE('',*,*,#5424,.T.);
#7331=ORIENTED_EDGE('',*,*,#5426,.F.);
#7332=ORIENTED_EDGE('',*,*,#5427,.F.);
#7333=ORIENTED_EDGE('',*,*,#5428,.T.);
#7334=ORIENTED_EDGE('',*,*,#5425,.T.);
#7335=ORIENTED_EDGE('',*,*,#5428,.F.);
#7336=ORIENTED_EDGE('',*,*,#5429,.F.);
#7337=ORIENTED_EDGE('',*,*,#5430,.T.);
#7338=ORIENTED_EDGE('',*,*,#5427,.T.);
#7339=ORIENTED_EDGE('',*,*,#5430,.F.);
#7340=ORIENTED_EDGE('',*,*,#5429,.T.);
#7341=ORIENTED_EDGE('',*,*,#5431,.T.);
#7342=ORIENTED_EDGE('',*,*,#5432,.T.);
#7343=ORIENTED_EDGE('',*,*,#5433,.T.);
#7344=ORIENTED_EDGE('',*,*,#5434,.F.);
#7345=ORIENTED_EDGE('',*,*,#5435,.T.);
#7346=ORIENTED_EDGE('',*,*,#5436,.T.);
#7347=ORIENTED_EDGE('',*,*,#5437,.T.);
#7348=ORIENTED_EDGE('',*,*,#5432,.F.);
#7349=ORIENTED_EDGE('',*,*,#5438,.T.);
#7350=ORIENTED_EDGE('',*,*,#5439,.T.);
#7351=ORIENTED_EDGE('',*,*,#5440,.T.);
#7352=ORIENTED_EDGE('',*,*,#5436,.F.);
#7353=ORIENTED_EDGE('',*,*,#5441,.T.);
#7354=ORIENTED_EDGE('',*,*,#5442,.T.);
#7355=ORIENTED_EDGE('',*,*,#5443,.T.);
#7356=ORIENTED_EDGE('',*,*,#5439,.F.);
#7357=ORIENTED_EDGE('',*,*,#5444,.T.);
#7358=ORIENTED_EDGE('',*,*,#5445,.T.);
#7359=ORIENTED_EDGE('',*,*,#5446,.T.);
#7360=ORIENTED_EDGE('',*,*,#5442,.F.);
#7361=ORIENTED_EDGE('',*,*,#5447,.T.);
#7362=ORIENTED_EDGE('',*,*,#5434,.T.);
#7363=ORIENTED_EDGE('',*,*,#5448,.T.);
#7364=ORIENTED_EDGE('',*,*,#5445,.F.);
#7365=ORIENTED_EDGE('',*,*,#5447,.F.);
#7366=ORIENTED_EDGE('',*,*,#5444,.F.);
#7367=ORIENTED_EDGE('',*,*,#5441,.F.);
#7368=ORIENTED_EDGE('',*,*,#5438,.F.);
#7369=ORIENTED_EDGE('',*,*,#5435,.F.);
#7370=ORIENTED_EDGE('',*,*,#5431,.F.);
#7371=ORIENTED_EDGE('',*,*,#5448,.F.);
#7372=ORIENTED_EDGE('',*,*,#5433,.F.);
#7373=ORIENTED_EDGE('',*,*,#5437,.F.);
#7374=ORIENTED_EDGE('',*,*,#5440,.F.);
#7375=ORIENTED_EDGE('',*,*,#5443,.F.);
#7376=ORIENTED_EDGE('',*,*,#5446,.F.);
#7377=ORIENTED_EDGE('',*,*,#5449,.F.);
#7378=ORIENTED_EDGE('',*,*,#5450,.T.);
#7379=ORIENTED_EDGE('',*,*,#5451,.F.);
#7380=ORIENTED_EDGE('',*,*,#5450,.F.);
#7381=ORIENTED_EDGE('',*,*,#5452,.F.);
#7382=ORIENTED_EDGE('',*,*,#5453,.T.);
#7383=ORIENTED_EDGE('',*,*,#5454,.F.);
#7384=ORIENTED_EDGE('',*,*,#5453,.F.);
#7385=ORIENTED_EDGE('',*,*,#5455,.F.);
#7386=ORIENTED_EDGE('',*,*,#5456,.F.);
#7387=ORIENTED_EDGE('',*,*,#5457,.F.);
#7388=ORIENTED_EDGE('',*,*,#5458,.T.);
#7389=ORIENTED_EDGE('',*,*,#5455,.T.);
#7390=ORIENTED_EDGE('',*,*,#5459,.T.);
#7391=ORIENTED_EDGE('',*,*,#5460,.F.);
#7392=ORIENTED_EDGE('',*,*,#5461,.F.);
#7393=ORIENTED_EDGE('',*,*,#5458,.F.);
#7394=ORIENTED_EDGE('',*,*,#5462,.F.);
#7395=ORIENTED_EDGE('',*,*,#5463,.F.);
#7396=ORIENTED_EDGE('',*,*,#5459,.F.);
#7397=ORIENTED_EDGE('',*,*,#5449,.T.);
#7398=ORIENTED_EDGE('',*,*,#5452,.T.);
#7399=ORIENTED_EDGE('',*,*,#5457,.T.);
#7400=ORIENTED_EDGE('',*,*,#5464,.F.);
#7401=ORIENTED_EDGE('',*,*,#5465,.F.);
#7402=ORIENTED_EDGE('',*,*,#5462,.T.);
#7403=ORIENTED_EDGE('',*,*,#5460,.T.);
#7404=ORIENTED_EDGE('',*,*,#5463,.T.);
#7405=ORIENTED_EDGE('',*,*,#5465,.T.);
#7406=ORIENTED_EDGE('',*,*,#5466,.F.);
#7407=ORIENTED_EDGE('',*,*,#5461,.T.);
#7408=ORIENTED_EDGE('',*,*,#5466,.T.);
#7409=ORIENTED_EDGE('',*,*,#5464,.T.);
#7410=ORIENTED_EDGE('',*,*,#5456,.T.);
#7411=ORIENTED_EDGE('',*,*,#5451,.T.);
#7412=ORIENTED_EDGE('',*,*,#5454,.T.);
#7413=ORIENTED_EDGE('',*,*,#5467,.F.);
#7414=ORIENTED_EDGE('',*,*,#5468,.T.);
#7415=ORIENTED_EDGE('',*,*,#5469,.T.);
#7416=ORIENTED_EDGE('',*,*,#5468,.F.);
#7417=ORIENTED_EDGE('',*,*,#5470,.F.);
#7418=ORIENTED_EDGE('',*,*,#5471,.T.);
#7419=ORIENTED_EDGE('',*,*,#5472,.T.);
#7420=ORIENTED_EDGE('',*,*,#5471,.F.);
#7421=ORIENTED_EDGE('',*,*,#5470,.T.);
#7422=ORIENTED_EDGE('',*,*,#5467,.T.);
#7423=ORIENTED_EDGE('',*,*,#5472,.F.);
#7424=ORIENTED_EDGE('',*,*,#5469,.F.);
#7425=ORIENTED_EDGE('',*,*,#5473,.F.);
#7426=ORIENTED_EDGE('',*,*,#5474,.T.);
#7427=ORIENTED_EDGE('',*,*,#5475,.T.);
#7428=ORIENTED_EDGE('',*,*,#5474,.F.);
#7429=ORIENTED_EDGE('',*,*,#5476,.F.);
#7430=ORIENTED_EDGE('',*,*,#5477,.T.);
#7431=ORIENTED_EDGE('',*,*,#5478,.T.);
#7432=ORIENTED_EDGE('',*,*,#5477,.F.);
#7433=ORIENTED_EDGE('',*,*,#5476,.T.);
#7434=ORIENTED_EDGE('',*,*,#5473,.T.);
#7435=ORIENTED_EDGE('',*,*,#5478,.F.);
#7436=ORIENTED_EDGE('',*,*,#5475,.F.);
#7437=ORIENTED_EDGE('',*,*,#5479,.F.);
#7438=ORIENTED_EDGE('',*,*,#5480,.T.);
#7439=ORIENTED_EDGE('',*,*,#5481,.T.);
#7440=ORIENTED_EDGE('',*,*,#5480,.F.);
#7441=ORIENTED_EDGE('',*,*,#5481,.F.);
#7442=ORIENTED_EDGE('',*,*,#5482,.F.);
#7443=ORIENTED_EDGE('',*,*,#5483,.F.);
#7444=ORIENTED_EDGE('',*,*,#5484,.F.);
#7445=ORIENTED_EDGE('',*,*,#5485,.F.);
#7446=ORIENTED_EDGE('',*,*,#5479,.T.);
#7447=ORIENTED_EDGE('',*,*,#5484,.T.);
#7448=ORIENTED_EDGE('',*,*,#5486,.T.);
#7449=ORIENTED_EDGE('',*,*,#5487,.F.);
#7450=ORIENTED_EDGE('',*,*,#5488,.F.);
#7451=ORIENTED_EDGE('',*,*,#5489,.T.);
#7452=ORIENTED_EDGE('',*,*,#5490,.F.);
#7453=ORIENTED_EDGE('',*,*,#5483,.T.);
#7454=ORIENTED_EDGE('',*,*,#5491,.F.);
#7455=ORIENTED_EDGE('',*,*,#5492,.F.);
#7456=ORIENTED_EDGE('',*,*,#5486,.F.);
#7457=ORIENTED_EDGE('',*,*,#5482,.T.);
#7458=ORIENTED_EDGE('',*,*,#5493,.F.);
#7459=ORIENTED_EDGE('',*,*,#5494,.F.);
#7460=ORIENTED_EDGE('',*,*,#5495,.F.);
#7461=ORIENTED_EDGE('',*,*,#5496,.F.);
#7462=ORIENTED_EDGE('',*,*,#5491,.T.);
#7463=ORIENTED_EDGE('',*,*,#5497,.F.);
#7464=ORIENTED_EDGE('',*,*,#5498,.F.);
#7465=ORIENTED_EDGE('',*,*,#5489,.F.);
#7466=ORIENTED_EDGE('',*,*,#5499,.F.);
#7467=ORIENTED_EDGE('',*,*,#5500,.F.);
#7468=ORIENTED_EDGE('',*,*,#5494,.T.);
#7469=ORIENTED_EDGE('',*,*,#5501,.F.);
#7470=ORIENTED_EDGE('',*,*,#5502,.F.);
#7471=ORIENTED_EDGE('',*,*,#5485,.T.);
#7472=ORIENTED_EDGE('',*,*,#5490,.T.);
#7473=ORIENTED_EDGE('',*,*,#5498,.T.);
#7474=ORIENTED_EDGE('',*,*,#5503,.F.);
#7475=ORIENTED_EDGE('',*,*,#5501,.T.);
#7476=ORIENTED_EDGE('',*,*,#5493,.T.);
#7477=ORIENTED_EDGE('',*,*,#5504,.F.);
#7478=ORIENTED_EDGE('',*,*,#5505,.T.);
#7479=ORIENTED_EDGE('',*,*,#5503,.T.);
#7480=ORIENTED_EDGE('',*,*,#5497,.T.);
#7481=ORIENTED_EDGE('',*,*,#5506,.T.);
#7482=ORIENTED_EDGE('',*,*,#5502,.T.);
#7483=ORIENTED_EDGE('',*,*,#5505,.F.);
#7484=ORIENTED_EDGE('',*,*,#5495,.T.);
#7485=ORIENTED_EDGE('',*,*,#5500,.T.);
#7486=ORIENTED_EDGE('',*,*,#5506,.F.);
#7487=ORIENTED_EDGE('',*,*,#5499,.T.);
#7488=ORIENTED_EDGE('',*,*,#5488,.T.);
#7489=ORIENTED_EDGE('',*,*,#5507,.T.);
#7490=ORIENTED_EDGE('',*,*,#5508,.T.);
#7491=ORIENTED_EDGE('',*,*,#5496,.T.);
#7492=ORIENTED_EDGE('',*,*,#5508,.F.);
#7493=ORIENTED_EDGE('',*,*,#5509,.T.);
#7494=ORIENTED_EDGE('',*,*,#5510,.T.);
#7495=ORIENTED_EDGE('',*,*,#5509,.F.);
#7496=ORIENTED_EDGE('',*,*,#5507,.F.);
#7497=ORIENTED_EDGE('',*,*,#5487,.T.);
#7498=ORIENTED_EDGE('',*,*,#5492,.T.);
#7499=ORIENTED_EDGE('',*,*,#5510,.F.);
#7500=ORIENTED_EDGE('',*,*,#5504,.T.);
#7501=ORIENTED_EDGE('',*,*,#5511,.F.);
#7502=ORIENTED_EDGE('',*,*,#5512,.T.);
#7503=ORIENTED_EDGE('',*,*,#5513,.F.);
#7504=ORIENTED_EDGE('',*,*,#5514,.F.);
#7505=ORIENTED_EDGE('',*,*,#5515,.T.);
#7506=ORIENTED_EDGE('',*,*,#5516,.F.);
#7507=ORIENTED_EDGE('',*,*,#5515,.F.);
#7508=ORIENTED_EDGE('',*,*,#5517,.F.);
#7509=ORIENTED_EDGE('',*,*,#5518,.F.);
#7510=ORIENTED_EDGE('',*,*,#5512,.F.);
#7511=ORIENTED_EDGE('',*,*,#5519,.F.);
#7512=ORIENTED_EDGE('',*,*,#5517,.T.);
#7513=ORIENTED_EDGE('',*,*,#5514,.T.);
#7514=ORIENTED_EDGE('',*,*,#5520,.F.);
#7515=ORIENTED_EDGE('',*,*,#5521,.T.);
#7516=ORIENTED_EDGE('',*,*,#5522,.F.);
#7517=ORIENTED_EDGE('',*,*,#5521,.F.);
#7518=ORIENTED_EDGE('',*,*,#5518,.T.);
#7519=ORIENTED_EDGE('',*,*,#5519,.T.);
#7520=ORIENTED_EDGE('',*,*,#5513,.T.);
#7521=ORIENTED_EDGE('',*,*,#5511,.T.);
#7522=ORIENTED_EDGE('',*,*,#5523,.T.);
#7523=ORIENTED_EDGE('',*,*,#5524,.T.);
#7524=ORIENTED_EDGE('',*,*,#5525,.F.);
#7525=ORIENTED_EDGE('',*,*,#5526,.F.);
#7526=ORIENTED_EDGE('',*,*,#5520,.T.);
#7527=ORIENTED_EDGE('',*,*,#5527,.T.);
#7528=ORIENTED_EDGE('',*,*,#5528,.T.);
#7529=ORIENTED_EDGE('',*,*,#5526,.T.);
#7530=ORIENTED_EDGE('',*,*,#5529,.F.);
#7531=ORIENTED_EDGE('',*,*,#5530,.T.);
#7532=ORIENTED_EDGE('',*,*,#5529,.T.);
#7533=ORIENTED_EDGE('',*,*,#5525,.T.);
#7534=ORIENTED_EDGE('',*,*,#5531,.T.);
#7535=ORIENTED_EDGE('',*,*,#5532,.T.);
#7536=ORIENTED_EDGE('',*,*,#5533,.F.);
#7537=ORIENTED_EDGE('',*,*,#5523,.F.);
#7538=ORIENTED_EDGE('',*,*,#5528,.F.);
#7539=ORIENTED_EDGE('',*,*,#5534,.T.);
#7540=ORIENTED_EDGE('',*,*,#5531,.F.);
#7541=ORIENTED_EDGE('',*,*,#5524,.F.);
#7542=ORIENTED_EDGE('',*,*,#5533,.T.);
#7543=ORIENTED_EDGE('',*,*,#5516,.T.);
#7544=ORIENTED_EDGE('',*,*,#5527,.F.);
#7545=ORIENTED_EDGE('',*,*,#5530,.F.);
#7546=ORIENTED_EDGE('',*,*,#5534,.F.);
#7547=ORIENTED_EDGE('',*,*,#5532,.F.);
#7548=ORIENTED_EDGE('',*,*,#5522,.T.);
#7549=ORIENTED_EDGE('',*,*,#5535,.T.);
#7550=ORIENTED_EDGE('',*,*,#5536,.F.);
#7551=ORIENTED_EDGE('',*,*,#5535,.F.);
#7552=ORIENTED_EDGE('',*,*,#5537,.T.);
#7553=ORIENTED_EDGE('',*,*,#5538,.T.);
#7554=ORIENTED_EDGE('',*,*,#5537,.F.);
#7555=ORIENTED_EDGE('',*,*,#5538,.F.);
#7556=ORIENTED_EDGE('',*,*,#5539,.F.);
#7557=ORIENTED_EDGE('',*,*,#5540,.T.);
#7558=ORIENTED_EDGE('',*,*,#5536,.T.);
#7559=ORIENTED_EDGE('',*,*,#5540,.F.);
#7560=ORIENTED_EDGE('',*,*,#5539,.T.);
#7561=ORIENTED_EDGE('',*,*,#5541,.F.);
#7562=ORIENTED_EDGE('',*,*,#5542,.T.);
#7563=ORIENTED_EDGE('',*,*,#5543,.T.);
#7564=ORIENTED_EDGE('',*,*,#5542,.F.);
#7565=ORIENTED_EDGE('',*,*,#5541,.T.);
#7566=ORIENTED_EDGE('',*,*,#5543,.F.);
#7567=ORIENTED_EDGE('',*,*,#5544,.F.);
#7568=ORIENTED_EDGE('',*,*,#5545,.T.);
#7569=ORIENTED_EDGE('',*,*,#5546,.T.);
#7570=ORIENTED_EDGE('',*,*,#5547,.F.);
#7571=ORIENTED_EDGE('',*,*,#5548,.F.);
#7572=ORIENTED_EDGE('',*,*,#5549,.T.);
#7573=ORIENTED_EDGE('',*,*,#5550,.T.);
#7574=ORIENTED_EDGE('',*,*,#5545,.F.);
#7575=ORIENTED_EDGE('',*,*,#5551,.F.);
#7576=ORIENTED_EDGE('',*,*,#5552,.T.);
#7577=ORIENTED_EDGE('',*,*,#5553,.T.);
#7578=ORIENTED_EDGE('',*,*,#5549,.F.);
#7579=ORIENTED_EDGE('',*,*,#5554,.F.);
#7580=ORIENTED_EDGE('',*,*,#5555,.T.);
#7581=ORIENTED_EDGE('',*,*,#5556,.T.);
#7582=ORIENTED_EDGE('',*,*,#5552,.F.);
#7583=ORIENTED_EDGE('',*,*,#5557,.F.);
#7584=ORIENTED_EDGE('',*,*,#5558,.T.);
#7585=ORIENTED_EDGE('',*,*,#5559,.T.);
#7586=ORIENTED_EDGE('',*,*,#5555,.F.);
#7587=ORIENTED_EDGE('',*,*,#5560,.F.);
#7588=ORIENTED_EDGE('',*,*,#5547,.T.);
#7589=ORIENTED_EDGE('',*,*,#5561,.T.);
#7590=ORIENTED_EDGE('',*,*,#5558,.F.);
#7591=ORIENTED_EDGE('',*,*,#5561,.F.);
#7592=ORIENTED_EDGE('',*,*,#5546,.F.);
#7593=ORIENTED_EDGE('',*,*,#5550,.F.);
#7594=ORIENTED_EDGE('',*,*,#5553,.F.);
#7595=ORIENTED_EDGE('',*,*,#5556,.F.);
#7596=ORIENTED_EDGE('',*,*,#5559,.F.);
#7597=ORIENTED_EDGE('',*,*,#5562,.F.);
#7598=ORIENTED_EDGE('',*,*,#5544,.T.);
#7599=ORIENTED_EDGE('',*,*,#5560,.T.);
#7600=ORIENTED_EDGE('',*,*,#5557,.T.);
#7601=ORIENTED_EDGE('',*,*,#5554,.T.);
#7602=ORIENTED_EDGE('',*,*,#5551,.T.);
#7603=ORIENTED_EDGE('',*,*,#5548,.T.);
#7604=ORIENTED_EDGE('',*,*,#5563,.F.);
#7605=ORIENTED_EDGE('',*,*,#5564,.T.);
#7606=ORIENTED_EDGE('',*,*,#5562,.T.);
#7607=ORIENTED_EDGE('',*,*,#5564,.F.);
#7608=ORIENTED_EDGE('',*,*,#5565,.F.);
#7609=ORIENTED_EDGE('',*,*,#5566,.T.);
#7610=ORIENTED_EDGE('',*,*,#5563,.T.);
#7611=ORIENTED_EDGE('',*,*,#5566,.F.);
#7612=ORIENTED_EDGE('',*,*,#5567,.F.);
#7613=ORIENTED_EDGE('',*,*,#5568,.T.);
#7614=ORIENTED_EDGE('',*,*,#5565,.T.);
#7615=ORIENTED_EDGE('',*,*,#5568,.F.);
#7616=ORIENTED_EDGE('',*,*,#5567,.T.);
#7617=CYLINDRICAL_SURFACE('',#8766,0.225);
#7618=CYLINDRICAL_SURFACE('',#8769,0.225);
#7619=CYLINDRICAL_SURFACE('',#8772,0.225);
#7620=CYLINDRICAL_SURFACE('',#8775,0.225);
#7621=CYLINDRICAL_SURFACE('',#8778,0.21);
#7622=CYLINDRICAL_SURFACE('',#8781,0.210000000000001);
#7623=CYLINDRICAL_SURFACE('',#8784,0.210000000000001);
#7624=CYLINDRICAL_SURFACE('',#8787,0.21);
#7625=CYLINDRICAL_SURFACE('',#8790,0.275);
#7626=CYLINDRICAL_SURFACE('',#8793,0.275);
#7627=CYLINDRICAL_SURFACE('',#8796,0.275);
#7628=CYLINDRICAL_SURFACE('',#8799,0.275);
#7629=CYLINDRICAL_SURFACE('',#8809,0.275);
#7630=CYLINDRICAL_SURFACE('',#8812,0.275);
#7631=CYLINDRICAL_SURFACE('',#8815,0.275);
#7632=CYLINDRICAL_SURFACE('',#8818,0.275);
#7633=CYLINDRICAL_SURFACE('',#8842,0.225);
#7634=CYLINDRICAL_SURFACE('',#8845,0.165);
#7635=CYLINDRICAL_SURFACE('',#8849,0.165);
#7636=CYLINDRICAL_SURFACE('',#8853,0.165);
#7637=CYLINDRICAL_SURFACE('',#8857,0.165);
#7638=CYLINDRICAL_SURFACE('',#8861,0.165);
#7639=CYLINDRICAL_SURFACE('',#8864,0.165);
#7640=CYLINDRICAL_SURFACE('',#8867,0.165);
#7641=CYLINDRICAL_SURFACE('',#8870,0.165);
#7642=CYLINDRICAL_SURFACE('',#8873,0.275);
#7643=CYLINDRICAL_SURFACE('',#8876,0.275);
#7644=CYLINDRICAL_SURFACE('',#8879,0.275);
#7645=CYLINDRICAL_SURFACE('',#8882,0.275);
#7646=CYLINDRICAL_SURFACE('',#8885,1.05);
#7647=CYLINDRICAL_SURFACE('',#8890,0.625);
#7648=CYLINDRICAL_SURFACE('',#8892,1.5);
#7649=CYLINDRICAL_SURFACE('',#8895,2.);
#7650=CYLINDRICAL_SURFACE('',#8907,2.2);
#7651=CYLINDRICAL_SURFACE('',#8917,0.225);
#7652=CYLINDRICAL_SURFACE('',#8920,0.225);
#7653=CYLINDRICAL_SURFACE('',#8923,0.225);
#7654=CYLINDRICAL_SURFACE('',#8926,0.225);
#7655=CYLINDRICAL_SURFACE('',#8929,1.49);
#7656=CYLINDRICAL_SURFACE('',#8934,0.71);
#7657=CYLINDRICAL_SURFACE('',#8936,2.2);
#7658=CYLINDRICAL_SURFACE('',#8942,0.225);
#7659=CYLINDRICAL_SURFACE('',#8945,0.225);
#7660=CYLINDRICAL_SURFACE('',#8948,0.225);
#7661=CYLINDRICAL_SURFACE('',#8951,0.225);
#7662=CYLINDRICAL_SURFACE('',#8954,1.49);
#7663=CYLINDRICAL_SURFACE('',#8959,0.71);
#7664=CYLINDRICAL_SURFACE('',#8961,2.2);
#7665=CYLINDRICAL_SURFACE('',#8967,0.375);
#7666=CYLINDRICAL_SURFACE('',#8972,0.375);
#7667=CYLINDRICAL_SURFACE('',#8977,0.375);
#7668=CYLINDRICAL_SURFACE('',#8982,0.375);
#7669=CYLINDRICAL_SURFACE('',#8987,0.225);
#7670=CYLINDRICAL_SURFACE('',#8989,0.225);
#7671=CYLINDRICAL_SURFACE('',#8991,0.225);
#7672=CYLINDRICAL_SURFACE('',#8993,0.225);
#7673=CYLINDRICAL_SURFACE('',#8995,1.04);
#7674=CYLINDRICAL_SURFACE('',#9000,0.625);
#7675=CYLINDRICAL_SURFACE('',#9002,2.);
#7676=CYLINDRICAL_SURFACE('',#9015,0.165);
#7677=CYLINDRICAL_SURFACE('',#9019,0.165);
#7678=CYLINDRICAL_SURFACE('',#9030,0.165);
#7679=CYLINDRICAL_SURFACE('',#9034,0.165);
#7680=CYLINDRICAL_SURFACE('',#9045,0.165);
#7681=CYLINDRICAL_SURFACE('',#9052,0.5);
#7682=CYLINDRICAL_SURFACE('',#9055,0.3);
#7683=CYLINDRICAL_SURFACE('',#9095,0.21);
#7684=CYLINDRICAL_SURFACE('',#9120,0.2117);
#7685=CYLINDRICAL_SURFACE('',#9133,0.265);
#7686=CYLINDRICAL_SURFACE('',#9137,0.5);
#7687=CYLINDRICAL_SURFACE('',#9155,0.425);
#7688=CYLINDRICAL_SURFACE('',#9163,0.24505);
#7689=CYLINDRICAL_SURFACE('',#9172,0.976185);
#7690=CYLINDRICAL_SURFACE('',#9174,0.5);
#7691=CYLINDRICAL_SURFACE('',#9180,0.976185);
#7692=CYLINDRICAL_SURFACE('',#9192,1.023815);
#7693=CYLINDRICAL_SURFACE('',#9199,1.5);
#7694=CYLINDRICAL_SURFACE('',#9204,1.023815);
#7695=CYLINDRICAL_SURFACE('',#9226,1.019052);
#7696=CYLINDRICAL_SURFACE('',#9266,0.980948);
#7697=CYLINDRICAL_SURFACE('',#9280,1.013815);
#7698=CYLINDRICAL_SURFACE('',#9284,0.991185);
#7699=CYLINDRICAL_SURFACE('',#9288,1.013815);
#7700=CYLINDRICAL_SURFACE('',#9292,0.991185);
#7701=CYLINDRICAL_SURFACE('',#9310,1.05);
#7702=CYLINDRICAL_SURFACE('',#9314,1.);
#7703=CYLINDRICAL_SURFACE('',#9318,1.05);
#7704=CYLINDRICAL_SURFACE('',#9322,1.);
#7705=CYLINDRICAL_SURFACE('',#9326,1.05);
#7706=CYLINDRICAL_SURFACE('',#9330,0.9);
#7707=CYLINDRICAL_SURFACE('',#9343,0.895);
#7708=CYLINDRICAL_SURFACE('',#9347,0.605);
#7709=CYLINDRICAL_SURFACE('',#9362,0.2);
#7710=CYLINDRICAL_SURFACE('',#9369,0.35);
#7711=CYLINDRICAL_SURFACE('',#9377,0.1954);
#7712=CYLINDRICAL_SURFACE('',#9382,0.305);
#7713=CYLINDRICAL_SURFACE('',#9385,0.8);
#7714=CYLINDRICAL_SURFACE('',#9398,0.7);
#7715=CYLINDRICAL_SURFACE('',#9407,1.);
#7716=CYLINDRICAL_SURFACE('',#9411,0.7);
#7717=CYLINDRICAL_SURFACE('',#9412,0.5);
#7718=CYLINDRICAL_SURFACE('',#9414,0.5);
#7719=CYLINDRICAL_SURFACE('',#9419,0.505);
#7720=CYLINDRICAL_SURFACE('',#9422,0.7);
#7721=CYLINDRICAL_SURFACE('',#9430,0.164999999999999);
#7722=CYLINDRICAL_SURFACE('',#9434,0.505);
#7723=CYLINDRICAL_SURFACE('',#9437,0.9);
#7724=CYLINDRICAL_SURFACE('',#9443,0.165);
#7725=CYLINDRICAL_SURFACE('',#9447,0.165);
#7726=CYLINDRICAL_SURFACE('',#9457,0.7);
#7727=CYLINDRICAL_SURFACE('',#9458,0.3);
#7728=CYLINDRICAL_SURFACE('',#9460,0.3);
#7729=CYLINDRICAL_SURFACE('',#9465,0.305);
#7730=CYLINDRICAL_SURFACE('',#9468,0.5);
#7731=CYLINDRICAL_SURFACE('',#9474,0.305);
#7732=CYLINDRICAL_SURFACE('',#9477,0.5);
#7733=CYLINDRICAL_SURFACE('',#9483,0.225);
#7734=CYLINDRICAL_SURFACE('',#9486,0.5);
#7735=CYLINDRICAL_SURFACE('',#9492,0.225);
#7736=CYLINDRICAL_SURFACE('',#9495,0.5);
#7737=CYLINDRICAL_SURFACE('',#9514,0.1954);
#7738=CYLINDRICAL_SURFACE('',#9530,0.35);
#7739=CYLINDRICAL_SURFACE('',#9538,0.1954);
#7740=CYLINDRICAL_SURFACE('',#9544,0.35);
#7741=CYLINDRICAL_SURFACE('',#9552,0.1954);
#7742=CYLINDRICAL_SURFACE('',#9635,0.5);
#7743=CYLINDRICAL_SURFACE('',#9638,0.5);
#7744=CYLINDRICAL_SURFACE('',#9641,0.8);
#7745=CYLINDRICAL_SURFACE('',#9648,0.8);
#7746=CYLINDRICAL_SURFACE('',#9652,0.305);
#7747=CYLINDRICAL_SURFACE('',#9655,0.5);
#7748=CYLINDRICAL_SURFACE('',#9661,0.305);
#7749=CYLINDRICAL_SURFACE('',#9664,0.5);
#7750=CYLINDRICAL_SURFACE('',#9674,0.305);
#7751=CYLINDRICAL_SURFACE('',#9687,0.6);
#7752=CYLINDRICAL_SURFACE('',#9693,1.2);
#7753=CYLINDRICAL_SURFACE('',#9699,0.165);
#7754=CYLINDRICAL_SURFACE('',#9704,0.305);
#7755=CYLINDRICAL_SURFACE('',#9717,0.5);
#7756=CYLINDRICAL_SURFACE('',#9720,0.3);
#7757=CYLINDRICAL_SURFACE('',#9724,1.);
#7758=CYLINDRICAL_SURFACE('',#9741,0.1954);
#7759=ADVANCED_FACE('',(#1087),#7617,.F.);
#7760=ADVANCED_FACE('',(#1088),#7618,.F.);
#7761=ADVANCED_FACE('',(#1089),#7619,.F.);
#7762=ADVANCED_FACE('',(#1090),#7620,.F.);
#7763=ADVANCED_FACE('',(#1091),#7621,.F.);
#7764=ADVANCED_FACE('',(#1092),#7622,.F.);
#7765=ADVANCED_FACE('',(#1093),#7623,.F.);
#7766=ADVANCED_FACE('',(#1094),#7624,.F.);
#7767=ADVANCED_FACE('',(#1095),#7625,.F.);
#7768=ADVANCED_FACE('',(#1096),#7626,.F.);
#7769=ADVANCED_FACE('',(#1097),#7627,.F.);
#7770=ADVANCED_FACE('',(#1098),#7628,.F.);
#7771=ADVANCED_FACE('',(#1099),#783,.T.);
#7772=ADVANCED_FACE('',(#1100),#784,.T.);
#7773=ADVANCED_FACE('',(#1101),#785,.T.);
#7774=ADVANCED_FACE('',(#1102),#786,.T.);
#7775=ADVANCED_FACE('',(#1103,#611,#612,#613,#614,#615,#616,#617,#618,#619,
#620,#621,#622),#787,.T.);
#7776=ADVANCED_FACE('',(#1104,#623,#624,#625,#626,#627,#628,#629,#630,#631,
#632,#633,#634),#788,.F.);
#7777=ADVANCED_FACE('',(#1105),#7629,.F.);
#7778=ADVANCED_FACE('',(#1106),#7630,.F.);
#7779=ADVANCED_FACE('',(#1107),#7631,.F.);
#7780=ADVANCED_FACE('',(#1108),#7632,.F.);
#7781=ADVANCED_FACE('',(#1109),#789,.T.);
#7782=ADVANCED_FACE('',(#1110),#790,.T.);
#7783=ADVANCED_FACE('',(#1111),#791,.T.);
#7784=ADVANCED_FACE('',(#1112),#792,.T.);
#7785=ADVANCED_FACE('',(#1113,#635,#636,#637,#638),#793,.T.);
#7786=ADVANCED_FACE('',(#1114,#639,#640,#641,#642),#794,.F.);
#7787=ADVANCED_FACE('',(#1115),#795,.T.);
#7788=ADVANCED_FACE('',(#1116),#796,.T.);
#7789=ADVANCED_FACE('',(#1117),#797,.T.);
#7790=ADVANCED_FACE('',(#1118),#798,.T.);
#7791=ADVANCED_FACE('',(#1119),#799,.T.);
#7792=ADVANCED_FACE('',(#1120),#800,.F.);
#7793=ADVANCED_FACE('',(#1121),#801,.T.);
#7794=ADVANCED_FACE('',(#1122),#802,.T.);
#7795=ADVANCED_FACE('',(#1123),#803,.T.);
#7796=ADVANCED_FACE('',(#1124),#804,.T.);
#7797=ADVANCED_FACE('',(#1125),#805,.T.);
#7798=ADVANCED_FACE('',(#1126),#806,.F.);
#7799=ADVANCED_FACE('',(#1127),#7633,.F.);
#7800=ADVANCED_FACE('',(#1128),#7634,.F.);
#7801=ADVANCED_FACE('',(#1129),#807,.T.);
#7802=ADVANCED_FACE('',(#1130),#7635,.F.);
#7803=ADVANCED_FACE('',(#1131),#808,.T.);
#7804=ADVANCED_FACE('',(#1132),#7636,.F.);
#7805=ADVANCED_FACE('',(#1133),#809,.T.);
#7806=ADVANCED_FACE('',(#1134),#7637,.F.);
#7807=ADVANCED_FACE('',(#1135),#810,.T.);
#7808=ADVANCED_FACE('',(#1136),#7638,.F.);
#7809=ADVANCED_FACE('',(#1137),#7639,.F.);
#7810=ADVANCED_FACE('',(#1138),#7640,.F.);
#7811=ADVANCED_FACE('',(#1139),#7641,.F.);
#7812=ADVANCED_FACE('',(#1140),#7642,.F.);
#7813=ADVANCED_FACE('',(#1141),#7643,.F.);
#7814=ADVANCED_FACE('',(#1142),#7644,.F.);
#7815=ADVANCED_FACE('',(#1143),#7645,.F.);
#7816=ADVANCED_FACE('',(#1144),#7646,.F.);
#7817=ADVANCED_FACE('',(#1145,#643),#811,.T.);
#7818=ADVANCED_FACE('',(#1146),#7647,.F.);
#7819=ADVANCED_FACE('',(#1147),#7648,.F.);
#7820=ADVANCED_FACE('',(#1148),#7649,.T.);
#7821=ADVANCED_FACE('',(#1149,#644,#645,#646,#647,#648,#649),#812,.T.);
#7822=ADVANCED_FACE('',(#1150,#650,#651,#652,#653,#654),#813,.T.);
#7823=ADVANCED_FACE('',(#1151,#655,#656,#657,#658,#659),#814,.T.);
#7824=ADVANCED_FACE('',(#1152),#815,.T.);
#7825=ADVANCED_FACE('',(#1153),#816,.T.);
#7826=ADVANCED_FACE('',(#1154),#817,.T.);
#7827=ADVANCED_FACE('',(#1155),#818,.T.);
#7828=ADVANCED_FACE('',(#1156),#819,.T.);
#7829=ADVANCED_FACE('',(#1157),#7650,.T.);
#7830=ADVANCED_FACE('',(#1158,#660,#661,#662,#663,#664,#665),#820,.T.);
#7831=ADVANCED_FACE('',(#1159),#821,.T.);
#7832=ADVANCED_FACE('',(#1160,#666),#822,.T.);
#7833=ADVANCED_FACE('',(#1161),#823,.T.);
#7834=ADVANCED_FACE('',(#1162),#824,.T.);
#7835=ADVANCED_FACE('',(#1163),#825,.T.);
#7836=ADVANCED_FACE('',(#1164,#667,#668,#669,#670),#826,.F.);
#7837=ADVANCED_FACE('',(#1165),#7651,.F.);
#7838=ADVANCED_FACE('',(#1166),#7652,.F.);
#7839=ADVANCED_FACE('',(#1167),#7653,.F.);
#7840=ADVANCED_FACE('',(#1168),#7654,.F.);
#7841=ADVANCED_FACE('',(#1169),#7655,.T.);
#7842=ADVANCED_FACE('',(#1170,#671),#827,.T.);
#7843=ADVANCED_FACE('',(#1171),#7656,.F.);
#7844=ADVANCED_FACE('',(#1172),#7657,.T.);
#7845=ADVANCED_FACE('',(#1173,#672,#673,#674,#675,#676),#828,.T.);
#7846=ADVANCED_FACE('',(#1174,#677,#678,#679,#680,#681),#829,.F.);
#7847=ADVANCED_FACE('',(#1175),#7658,.F.);
#7848=ADVANCED_FACE('',(#1176),#7659,.F.);
#7849=ADVANCED_FACE('',(#1177),#7660,.F.);
#7850=ADVANCED_FACE('',(#1178),#7661,.F.);
#7851=ADVANCED_FACE('',(#1179),#7662,.T.);
#7852=ADVANCED_FACE('',(#1180,#682),#830,.F.);
#7853=ADVANCED_FACE('',(#1181),#7663,.F.);
#7854=ADVANCED_FACE('',(#1182),#7664,.T.);
#7855=ADVANCED_FACE('',(#1183,#683,#684,#685,#686,#687),#831,.T.);
#7856=ADVANCED_FACE('',(#1184,#688,#689,#690,#691,#692),#832,.F.);
#7857=ADVANCED_FACE('',(#1185),#7665,.F.);
#7858=ADVANCED_FACE('',(#1186,#693),#833,.T.);
#7859=ADVANCED_FACE('',(#1187),#7666,.F.);
#7860=ADVANCED_FACE('',(#1188,#694),#834,.T.);
#7861=ADVANCED_FACE('',(#1189),#7667,.F.);
#7862=ADVANCED_FACE('',(#1190,#695),#835,.T.);
#7863=ADVANCED_FACE('',(#1191),#7668,.F.);
#7864=ADVANCED_FACE('',(#1192,#696),#836,.T.);
#7865=ADVANCED_FACE('',(#1193),#7669,.F.);
#7866=ADVANCED_FACE('',(#1194),#7670,.F.);
#7867=ADVANCED_FACE('',(#1195),#7671,.F.);
#7868=ADVANCED_FACE('',(#1196),#7672,.F.);
#7869=ADVANCED_FACE('',(#1197),#7673,.T.);
#7870=ADVANCED_FACE('',(#1198,#697),#837,.F.);
#7871=ADVANCED_FACE('',(#1199),#7674,.F.);
#7872=ADVANCED_FACE('',(#1200),#7675,.T.);
#7873=ADVANCED_FACE('',(#1201,#698,#699,#700,#701,#702),#838,.T.);
#7874=ADVANCED_FACE('',(#1202,#703,#704,#705,#706,#707),#839,.F.);
#7875=ADVANCED_FACE('',(#1203),#840,.T.);
#7876=ADVANCED_FACE('',(#1204),#841,.T.);
#7877=ADVANCED_FACE('',(#1205),#842,.T.);
#7878=ADVANCED_FACE('',(#1206),#843,.T.);
#7879=ADVANCED_FACE('',(#1207),#844,.T.);
#7880=ADVANCED_FACE('',(#1208),#845,.F.);
#7881=ADVANCED_FACE('',(#1209),#7676,.F.);
#7882=ADVANCED_FACE('',(#1210),#846,.F.);
#7883=ADVANCED_FACE('',(#1211),#7677,.F.);
#7884=ADVANCED_FACE('',(#1212),#847,.F.);
#7885=ADVANCED_FACE('',(#1213),#848,.T.);
#7886=ADVANCED_FACE('',(#1214),#849,.T.);
#7887=ADVANCED_FACE('',(#1215),#850,.T.);
#7888=ADVANCED_FACE('',(#1216),#851,.T.);
#7889=ADVANCED_FACE('',(#1217),#852,.T.);
#7890=ADVANCED_FACE('',(#1218,#708,#709),#853,.F.);
#7891=ADVANCED_FACE('',(#1219),#7678,.F.);
#7892=ADVANCED_FACE('',(#1220),#854,.F.);
#7893=ADVANCED_FACE('',(#1221),#7679,.F.);
#7894=ADVANCED_FACE('',(#1222),#855,.F.);
#7895=ADVANCED_FACE('',(#1223),#856,.T.);
#7896=ADVANCED_FACE('',(#1224),#857,.T.);
#7897=ADVANCED_FACE('',(#1225),#858,.T.);
#7898=ADVANCED_FACE('',(#1226),#859,.T.);
#7899=ADVANCED_FACE('',(#1227),#860,.T.);
#7900=ADVANCED_FACE('',(#1228,#710,#711),#861,.F.);
#7901=ADVANCED_FACE('',(#1229),#7680,.F.);
#7902=ADVANCED_FACE('',(#1230),#862,.T.);
#7903=ADVANCED_FACE('',(#1231,#712),#863,.F.);
#7904=ADVANCED_FACE('',(#1232),#7681,.T.);
#7905=ADVANCED_FACE('',(#1233,#713),#864,.T.);
#7906=ADVANCED_FACE('',(#1234),#7682,.T.);
#7907=ADVANCED_FACE('',(#1235),#865,.F.);
#7908=ADVANCED_FACE('',(#1236),#866,.F.);
#7909=ADVANCED_FACE('',(#1237),#867,.F.);
#7910=ADVANCED_FACE('',(#1238),#868,.F.);
#7911=ADVANCED_FACE('',(#1239),#869,.F.);
#7912=ADVANCED_FACE('',(#1240),#870,.F.);
#7913=ADVANCED_FACE('',(#1241),#871,.F.);
#7914=ADVANCED_FACE('',(#1242),#872,.F.);
#7915=ADVANCED_FACE('',(#1243),#873,.F.);
#7916=ADVANCED_FACE('',(#1244),#874,.F.);
#7917=ADVANCED_FACE('',(#1245),#875,.F.);
#7918=ADVANCED_FACE('',(#1246),#876,.F.);
#7919=ADVANCED_FACE('',(#1247),#877,.F.);
#7920=ADVANCED_FACE('',(#1248),#878,.F.);
#7921=ADVANCED_FACE('',(#1249),#879,.F.);
#7922=ADVANCED_FACE('',(#1250),#880,.F.);
#7923=ADVANCED_FACE('',(#1251),#881,.F.);
#7924=ADVANCED_FACE('',(#1252),#882,.F.);
#7925=ADVANCED_FACE('',(#1253),#883,.F.);
#7926=ADVANCED_FACE('',(#1254),#884,.F.);
#7927=ADVANCED_FACE('',(#1255),#885,.F.);
#7928=ADVANCED_FACE('',(#1256),#886,.F.);
#7929=ADVANCED_FACE('',(#1257),#887,.F.);
#7930=ADVANCED_FACE('',(#1258),#888,.F.);
#7931=ADVANCED_FACE('',(#1259),#889,.F.);
#7932=ADVANCED_FACE('',(#1260),#890,.F.);
#7933=ADVANCED_FACE('',(#1261),#891,.F.);
#7934=ADVANCED_FACE('',(#1262),#892,.F.);
#7935=ADVANCED_FACE('',(#1263),#893,.F.);
#7936=ADVANCED_FACE('',(#1264),#894,.F.);
#7937=ADVANCED_FACE('',(#1265),#895,.F.);
#7938=ADVANCED_FACE('',(#1266),#896,.F.);
#7939=ADVANCED_FACE('',(#1267),#897,.F.);
#7940=ADVANCED_FACE('',(#1268),#898,.F.);
#7941=ADVANCED_FACE('',(#1269),#899,.F.);
#7942=ADVANCED_FACE('',(#1270),#900,.F.);
#7943=ADVANCED_FACE('',(#1271),#901,.F.);
#7944=ADVANCED_FACE('',(#1272),#7683,.F.);
#7945=ADVANCED_FACE('',(#1273),#902,.T.);
#7946=ADVANCED_FACE('',(#1274),#903,.T.);
#7947=ADVANCED_FACE('',(#1275),#904,.T.);
#7948=ADVANCED_FACE('',(#1276),#905,.T.);
#7949=ADVANCED_FACE('',(#1277),#906,.T.);
#7950=ADVANCED_FACE('',(#1278),#907,.T.);
#7951=ADVANCED_FACE('',(#1279),#908,.T.);
#7952=ADVANCED_FACE('',(#1280),#909,.T.);
#7953=ADVANCED_FACE('',(#1281,#714),#910,.T.);
#7954=ADVANCED_FACE('',(#1282,#715),#911,.F.);
#7955=ADVANCED_FACE('',(#1283),#912,.F.);
#7956=ADVANCED_FACE('',(#1284),#913,.T.);
#7957=ADVANCED_FACE('',(#1285,#716),#914,.T.);
#7958=ADVANCED_FACE('',(#1286),#915,.T.);
#7959=ADVANCED_FACE('',(#1287),#916,.T.);
#7960=ADVANCED_FACE('',(#1288),#917,.F.);
#7961=ADVANCED_FACE('',(#1289),#918,.T.);
#7962=ADVANCED_FACE('',(#1290),#919,.T.);
#7963=ADVANCED_FACE('',(#1291),#920,.T.);
#7964=ADVANCED_FACE('',(#1292),#7684,.F.);
#7965=ADVANCED_FACE('',(#1293),#921,.F.);
#7966=ADVANCED_FACE('',(#1294),#922,.F.);
#7967=ADVANCED_FACE('',(#1295),#923,.T.);
#7968=ADVANCED_FACE('',(#1296),#924,.T.);
#7969=ADVANCED_FACE('',(#1297),#405,.F.);
#7970=ADVANCED_FACE('',(#1298),#7685,.F.);
#7971=ADVANCED_FACE('',(#1299,#717),#925,.T.);
#7972=ADVANCED_FACE('',(#1300),#7686,.T.);
#7973=ADVANCED_FACE('',(#1301,#718),#926,.F.);
#7974=ADVANCED_FACE('',(#1302),#927,.F.);
#7975=ADVANCED_FACE('',(#1303),#928,.F.);
#7976=ADVANCED_FACE('',(#1304),#929,.F.);
#7977=ADVANCED_FACE('',(#1305),#930,.F.);
#7978=ADVANCED_FACE('',(#1306),#931,.F.);
#7979=ADVANCED_FACE('',(#1307),#932,.F.);
#7980=ADVANCED_FACE('',(#1308),#933,.F.);
#7981=ADVANCED_FACE('',(#1309),#934,.F.);
#7982=ADVANCED_FACE('',(#1310),#935,.F.);
#7983=ADVANCED_FACE('',(#1311),#936,.T.);
#7984=ADVANCED_FACE('',(#1312),#406,.T.);
#7985=ADVANCED_FACE('',(#1313),#7687,.T.);
#7986=ADVANCED_FACE('',(#1314),#407,.T.);
#7987=ADVANCED_FACE('',(#1315,#719),#937,.T.);
#7988=ADVANCED_FACE('',(#1316),#408,.T.);
#7989=ADVANCED_FACE('',(#1317),#7688,.T.);
#7990=ADVANCED_FACE('',(#1318),#395,.F.);
#7991=ADVANCED_FACE('',(#1319),#7689,.T.);
#7992=ADVANCED_FACE('',(#1320),#7690,.F.);
#7993=ADVANCED_FACE('',(#1321),#409,.F.);
#7994=ADVANCED_FACE('',(#1322,#720),#938,.T.);
#7995=ADVANCED_FACE('',(#1323),#7691,.T.);
#7996=ADVANCED_FACE('',(#1324,#721),#939,.T.);
#7997=ADVANCED_FACE('',(#1325),#410,.F.);
#7998=ADVANCED_FACE('',(#1326),#396,.F.);
#7999=ADVANCED_FACE('',(#1327),#7692,.F.);
#8000=ADVANCED_FACE('',(#1328,#722),#940,.T.);
#8001=ADVANCED_FACE('',(#1329),#411,.T.);
#8002=ADVANCED_FACE('',(#1330),#7693,.T.);
#8003=ADVANCED_FACE('',(#1331),#412,.T.);
#8004=ADVANCED_FACE('',(#1332,#723),#941,.T.);
#8005=ADVANCED_FACE('',(#1333),#7694,.F.);
#8006=ADVANCED_FACE('',(#1334),#379,.T.);
#8007=ADVANCED_FACE('',(#1335),#380,.T.);
#8008=ADVANCED_FACE('',(#1336),#381,.T.);
#8009=ADVANCED_FACE('',(#1337),#382,.T.);
#8010=ADVANCED_FACE('',(#1338),#383,.T.);
#8011=ADVANCED_FACE('',(#1339),#384,.T.);
#8012=ADVANCED_FACE('',(#1340),#385,.T.);
#8013=ADVANCED_FACE('',(#1341),#386,.T.);
#8014=ADVANCED_FACE('',(#1342),#387,.F.);
#8015=ADVANCED_FACE('',(#1343),#7695,.T.);
#8016=ADVANCED_FACE('',(#1344),#942,.T.);
#8017=ADVANCED_FACE('',(#1345),#388,.F.);
#8018=ADVANCED_FACE('',(#1346),#943,.T.);
#8019=ADVANCED_FACE('',(#1347),#389,.F.);
#8020=ADVANCED_FACE('',(#1348),#944,.T.);
#8021=ADVANCED_FACE('',(#1349),#390,.F.);
#8022=ADVANCED_FACE('',(#1350),#945,.T.);
#8023=ADVANCED_FACE('',(#1351),#391,.F.);
#8024=ADVANCED_FACE('',(#1352),#946,.T.);
#8025=ADVANCED_FACE('',(#1353),#392,.F.);
#8026=ADVANCED_FACE('',(#1354),#947,.T.);
#8027=ADVANCED_FACE('',(#1355),#393,.F.);
#8028=ADVANCED_FACE('',(#1356),#7696,.F.);
#8029=ADVANCED_FACE('',(#1357),#948,.T.);
#8030=ADVANCED_FACE('',(#1358),#394,.F.);
#8031=ADVANCED_FACE('',(#1359,#724),#949,.T.);
#8032=ADVANCED_FACE('',(#1360),#950,.T.);
#8033=ADVANCED_FACE('',(#1361,#725),#951,.T.);
#8034=ADVANCED_FACE('',(#1362),#7697,.T.);
#8035=ADVANCED_FACE('',(#1363,#726),#952,.T.);
#8036=ADVANCED_FACE('',(#1364),#7698,.F.);
#8037=ADVANCED_FACE('',(#1365,#727),#953,.T.);
#8038=ADVANCED_FACE('',(#1366),#7699,.T.);
#8039=ADVANCED_FACE('',(#1367,#728),#954,.T.);
#8040=ADVANCED_FACE('',(#1368),#7700,.F.);
#8041=ADVANCED_FACE('',(#1369),#955,.F.);
#8042=ADVANCED_FACE('',(#1370),#956,.F.);
#8043=ADVANCED_FACE('',(#1371),#957,.F.);
#8044=ADVANCED_FACE('',(#1372),#958,.F.);
#8045=ADVANCED_FACE('',(#1373),#959,.F.);
#8046=ADVANCED_FACE('',(#1374,#729),#960,.T.);
#8047=ADVANCED_FACE('',(#1375),#7701,.T.);
#8048=ADVANCED_FACE('',(#1376,#730),#961,.T.);
#8049=ADVANCED_FACE('',(#1377),#7702,.T.);
#8050=ADVANCED_FACE('',(#1378,#731),#962,.T.);
#8051=ADVANCED_FACE('',(#1379),#7703,.T.);
#8052=ADVANCED_FACE('',(#1380,#732),#963,.T.);
#8053=ADVANCED_FACE('',(#1381),#7704,.T.);
#8054=ADVANCED_FACE('',(#1382,#733),#964,.T.);
#8055=ADVANCED_FACE('',(#1383),#7705,.T.);
#8056=ADVANCED_FACE('',(#1384,#734),#965,.T.);
#8057=ADVANCED_FACE('',(#1385,#735),#7706,.F.);
#8058=ADVANCED_FACE('',(#1386),#966,.F.);
#8059=ADVANCED_FACE('',(#1387),#967,.F.);
#8060=ADVANCED_FACE('',(#1388),#968,.F.);
#8061=ADVANCED_FACE('',(#1389),#969,.F.);
#8062=ADVANCED_FACE('',(#1390,#736),#970,.T.);
#8063=ADVANCED_FACE('',(#1391,#737),#7707,.T.);
#8064=ADVANCED_FACE('',(#1392,#738),#971,.T.);
#8065=ADVANCED_FACE('',(#1393,#739),#7708,.F.);
#8066=ADVANCED_FACE('',(#1394),#972,.F.);
#8067=ADVANCED_FACE('',(#1395),#973,.F.);
#8068=ADVANCED_FACE('',(#1396),#974,.F.);
#8069=ADVANCED_FACE('',(#1397),#975,.F.);
#8070=ADVANCED_FACE('',(#1398),#976,.F.);
#8071=ADVANCED_FACE('',(#1399),#977,.F.);
#8072=ADVANCED_FACE('',(#1400),#978,.F.);
#8073=ADVANCED_FACE('',(#1401),#979,.F.);
#8074=ADVANCED_FACE('',(#1402,#740),#980,.T.);
#8075=ADVANCED_FACE('',(#1403),#7709,.T.);
#8076=ADVANCED_FACE('',(#1404),#981,.F.);
#8077=ADVANCED_FACE('',(#1405),#982,.T.);
#8078=ADVANCED_FACE('',(#1406),#413,.T.);
#8079=ADVANCED_FACE('',(#1407),#7710,.T.);
#8080=ADVANCED_FACE('',(#1408),#414,.T.);
#8081=ADVANCED_FACE('',(#1409,#741),#983,.T.);
#8082=ADVANCED_FACE('',(#1410),#415,.T.);
#8083=ADVANCED_FACE('',(#1411),#7711,.T.);
#8084=ADVANCED_FACE('',(#1412),#416,.T.);
#8085=ADVANCED_FACE('',(#1413),#7712,.F.);
#8086=ADVANCED_FACE('',(#1414),#7713,.T.);
#8087=ADVANCED_FACE('',(#1415,#742,#743),#984,.F.);
#8088=ADVANCED_FACE('',(#1416),#985,.T.);
#8089=ADVANCED_FACE('',(#1417),#986,.T.);
#8090=ADVANCED_FACE('',(#1418),#987,.T.);
#8091=ADVANCED_FACE('',(#1419),#7714,.T.);
#8092=ADVANCED_FACE('',(#1420),#988,.T.);
#8093=ADVANCED_FACE('',(#1421,#744),#989,.T.);
#8094=ADVANCED_FACE('',(#1422),#990,.T.);
#8095=ADVANCED_FACE('',(#1423,#745),#991,.T.);
#8096=ADVANCED_FACE('',(#1424),#7715,.T.);
#8097=ADVANCED_FACE('',(#1425,#746),#992,.T.);
#8098=ADVANCED_FACE('',(#1426),#7716,.T.);
#8099=ADVANCED_FACE('',(#1427),#7717,.T.);
#8100=ADVANCED_FACE('',(#1428),#7718,.T.);
#8101=ADVANCED_FACE('',(#1429),#993,.T.);
#8102=ADVANCED_FACE('',(#1430),#994,.F.);
#8103=ADVANCED_FACE('',(#1431),#7719,.F.);
#8104=ADVANCED_FACE('',(#1432),#7720,.T.);
#8105=ADVANCED_FACE('',(#1433,#747),#995,.T.);
#8106=ADVANCED_FACE('',(#1434,#748),#996,.F.);
#8107=ADVANCED_FACE('',(#1435),#997,.T.);
#8108=ADVANCED_FACE('',(#1436),#7721,.F.);
#8109=ADVANCED_FACE('',(#1437),#998,.T.);
#8110=ADVANCED_FACE('',(#1438,#749),#7722,.F.);
#8111=ADVANCED_FACE('',(#1439,#750),#7723,.T.);
#8112=ADVANCED_FACE('',(#1440,#751),#999,.T.);
#8113=ADVANCED_FACE('',(#1441,#752),#1000,.F.);
#8114=ADVANCED_FACE('',(#1442),#7724,.F.);
#8115=ADVANCED_FACE('',(#1443),#1001,.T.);
#8116=ADVANCED_FACE('',(#1444),#7725,.F.);
#8117=ADVANCED_FACE('',(#1445),#1002,.F.);
#8118=ADVANCED_FACE('',(#1446,#753),#1003,.T.);
#8119=ADVANCED_FACE('',(#1447,#754),#1004,.F.);
#8120=ADVANCED_FACE('',(#1448),#7726,.T.);
#8121=ADVANCED_FACE('',(#1449),#7727,.T.);
#8122=ADVANCED_FACE('',(#1450),#7728,.T.);
#8123=ADVANCED_FACE('',(#1451,#755),#1005,.T.);
#8124=ADVANCED_FACE('',(#1452,#756),#1006,.F.);
#8125=ADVANCED_FACE('',(#1453),#7729,.F.);
#8126=ADVANCED_FACE('',(#1454),#7730,.T.);
#8127=ADVANCED_FACE('',(#1455,#757),#1007,.T.);
#8128=ADVANCED_FACE('',(#1456,#758),#1008,.F.);
#8129=ADVANCED_FACE('',(#1457),#7731,.F.);
#8130=ADVANCED_FACE('',(#1458),#7732,.T.);
#8131=ADVANCED_FACE('',(#1459,#759),#1009,.T.);
#8132=ADVANCED_FACE('',(#1460,#760),#1010,.F.);
#8133=ADVANCED_FACE('',(#1461),#7733,.F.);
#8134=ADVANCED_FACE('',(#1462),#7734,.T.);
#8135=ADVANCED_FACE('',(#1463,#761),#1011,.T.);
#8136=ADVANCED_FACE('',(#1464,#762),#1012,.F.);
#8137=ADVANCED_FACE('',(#1465),#7735,.F.);
#8138=ADVANCED_FACE('',(#1466),#7736,.T.);
#8139=ADVANCED_FACE('',(#1467,#763),#1013,.T.);
#8140=ADVANCED_FACE('',(#1468,#764),#1014,.F.);
#8141=ADVANCED_FACE('',(#1469),#1015,.F.);
#8142=ADVANCED_FACE('',(#1470),#1016,.F.);
#8143=ADVANCED_FACE('',(#1471),#1017,.F.);
#8144=ADVANCED_FACE('',(#1472),#1018,.F.);
#8145=ADVANCED_FACE('',(#1473),#1019,.F.);
#8146=ADVANCED_FACE('',(#1474),#1020,.F.);
#8147=ADVANCED_FACE('',(#1475),#1021,.F.);
#8148=ADVANCED_FACE('',(#1476),#1022,.F.);
#8149=ADVANCED_FACE('',(#1477,#765),#1023,.T.);
#8150=ADVANCED_FACE('',(#1478),#417,.T.);
#8151=ADVANCED_FACE('',(#1479),#7737,.T.);
#8152=ADVANCED_FACE('',(#1480),#1024,.F.);
#8153=ADVANCED_FACE('',(#1481),#1025,.F.);
#8154=ADVANCED_FACE('',(#1482),#1026,.F.);
#8155=ADVANCED_FACE('',(#1483),#1027,.F.);
#8156=ADVANCED_FACE('',(#1484),#1028,.F.);
#8157=ADVANCED_FACE('',(#1485),#1029,.F.);
#8158=ADVANCED_FACE('',(#1486),#1030,.F.);
#8159=ADVANCED_FACE('',(#1487),#1031,.F.);
#8160=ADVANCED_FACE('',(#1488),#1032,.F.);
#8161=ADVANCED_FACE('',(#1489),#1033,.T.);
#8162=ADVANCED_FACE('',(#1490),#418,.T.);
#8163=ADVANCED_FACE('',(#1491),#7738,.T.);
#8164=ADVANCED_FACE('',(#1492),#419,.T.);
#8165=ADVANCED_FACE('',(#1493,#766),#1034,.T.);
#8166=ADVANCED_FACE('',(#1494),#420,.T.);
#8167=ADVANCED_FACE('',(#1495),#7739,.T.);
#8168=ADVANCED_FACE('',(#1496),#1035,.T.);
#8169=ADVANCED_FACE('',(#1497),#421,.T.);
#8170=ADVANCED_FACE('',(#1498),#7740,.T.);
#8171=ADVANCED_FACE('',(#1499),#422,.T.);
#8172=ADVANCED_FACE('',(#1500,#767),#1036,.T.);
#8173=ADVANCED_FACE('',(#1501),#423,.T.);
#8174=ADVANCED_FACE('',(#1502),#7741,.T.);
#8175=ADVANCED_FACE('',(#1503),#424,.T.);
#8176=ADVANCED_FACE('',(#1504),#1037,.T.);
#8177=ADVANCED_FACE('',(#1505),#1038,.F.);
#8178=ADVANCED_FACE('',(#1506),#1039,.F.);
#8179=ADVANCED_FACE('',(#1507),#1040,.F.);
#8180=ADVANCED_FACE('',(#1508),#1041,.F.);
#8181=ADVANCED_FACE('',(#1509),#1042,.F.);
#8182=ADVANCED_FACE('',(#1510),#1043,.F.);
#8183=ADVANCED_FACE('',(#1511),#1044,.F.);
#8184=ADVANCED_FACE('',(#1512),#1045,.F.);
#8185=ADVANCED_FACE('',(#1513),#7742,.F.);
#8186=ADVANCED_FACE('',(#1514),#7743,.F.);
#8187=ADVANCED_FACE('',(#1515),#7744,.T.);
#8188=ADVANCED_FACE('',(#1516),#1046,.T.);
#8189=ADVANCED_FACE('',(#1517,#768,#769),#1047,.F.);
#8190=ADVANCED_FACE('',(#1518),#1048,.T.);
#8191=ADVANCED_FACE('',(#1519),#7745,.T.);
#8192=ADVANCED_FACE('',(#1520,#770,#771),#1049,.T.);
#8193=ADVANCED_FACE('',(#1521),#7746,.F.);
#8194=ADVANCED_FACE('',(#1522),#7747,.T.);
#8195=ADVANCED_FACE('',(#1523,#772),#1050,.T.);
#8196=ADVANCED_FACE('',(#1524,#773),#1051,.F.);
#8197=ADVANCED_FACE('',(#1525),#7748,.F.);
#8198=ADVANCED_FACE('',(#1526),#7749,.T.);
#8199=ADVANCED_FACE('',(#1527,#774),#1052,.T.);
#8200=ADVANCED_FACE('',(#1528,#775),#1053,.F.);
#8201=ADVANCED_FACE('',(#1529),#7750,.F.);
#8202=ADVANCED_FACE('',(#1530),#1054,.F.);
#8203=ADVANCED_FACE('',(#1531,#776),#1055,.F.);
#8204=ADVANCED_FACE('',(#1532),#1056,.T.);
#8205=ADVANCED_FACE('',(#1533),#1057,.F.);
#8206=ADVANCED_FACE('',(#1534),#1058,.T.);
#8207=ADVANCED_FACE('',(#1535),#1059,.T.);
#8208=ADVANCED_FACE('',(#1536),#1060,.T.);
#8209=ADVANCED_FACE('',(#1537),#1061,.T.);
#8210=ADVANCED_FACE('',(#1538),#7751,.T.);
#8211=ADVANCED_FACE('',(#1539),#1062,.T.);
#8212=ADVANCED_FACE('',(#1540),#7752,.T.);
#8213=ADVANCED_FACE('',(#1541),#1063,.F.);
#8214=ADVANCED_FACE('',(#1542),#1064,.T.);
#8215=ADVANCED_FACE('',(#1543),#1065,.T.);
#8216=ADVANCED_FACE('',(#1544),#7753,.F.);
#8217=ADVANCED_FACE('',(#1545),#1066,.T.);
#8218=ADVANCED_FACE('',(#1546,#777),#7754,.F.);
#8219=ADVANCED_FACE('',(#1547,#778),#1067,.T.);
#8220=ADVANCED_FACE('',(#1548),#1068,.T.);
#8221=ADVANCED_FACE('',(#1549),#1069,.T.);
#8222=ADVANCED_FACE('',(#1550),#1070,.F.);
#8223=ADVANCED_FACE('',(#1551,#779),#1071,.T.);
#8224=ADVANCED_FACE('',(#1552,#780),#1072,.T.);
#8225=ADVANCED_FACE('',(#1553,#781),#1073,.T.);
#8226=ADVANCED_FACE('',(#1554),#7755,.T.);
#8227=ADVANCED_FACE('',(#1555),#1074,.F.);
#8228=ADVANCED_FACE('',(#1556),#7756,.T.);
#8229=ADVANCED_FACE('',(#1557),#1075,.T.);
#8230=ADVANCED_FACE('',(#1558),#7757,.T.);
#8231=ADVANCED_FACE('',(#1559),#1076,.T.);
#8232=ADVANCED_FACE('',(#1560),#1077,.F.);
#8233=ADVANCED_FACE('',(#1561),#1078,.F.);
#8234=ADVANCED_FACE('',(#1562),#1079,.F.);
#8235=ADVANCED_FACE('',(#1563),#1080,.F.);
#8236=ADVANCED_FACE('',(#1564),#1081,.F.);
#8237=ADVANCED_FACE('',(#1565),#1082,.F.);
#8238=ADVANCED_FACE('',(#1566),#1083,.F.);
#8239=ADVANCED_FACE('',(#1567),#1084,.F.);
#8240=ADVANCED_FACE('',(#1568,#782),#1085,.T.);
#8241=ADVANCED_FACE('',(#1569),#425,.T.);
#8242=ADVANCED_FACE('',(#1570),#7758,.T.);
#8243=ADVANCED_FACE('',(#1571),#426,.T.);
#8244=ADVANCED_FACE('',(#1572),#1086,.T.);
#8245=CLOSED_SHELL('',(#7759,#7760,#7761,#7762,#7763,#7764,#7765,#7766,
#7767,#7768,#7769,#7770,#7771,#7772,#7773,#7774,#7775,#7776));
#8246=CLOSED_SHELL('',(#7777,#7778,#7779,#7780,#7781,#7782,#7783,#7784,
#7785,#7786));
#8247=CLOSED_SHELL('',(#7787,#7788,#7789,#7790,#7791,#7792));
#8248=CLOSED_SHELL('',(#7793,#7794,#7795,#7796,#7797,#7798));
#8249=CLOSED_SHELL('',(#7799,#7800,#7801,#7802,#7803,#7804,#7805,#7806,
#7807,#7808,#7809,#7810,#7811,#7812,#7813,#7814,#7815,#7816,#7817,#7818,
#7819,#7820,#7821,#7822,#7823,#7824,#7825,#7826,#7827,#7828,#7829,#7830,
#7831,#7832,#7833,#7834,#7835,#7836));
#8250=CLOSED_SHELL('',(#7837,#7838,#7839,#7840,#7841,#7842,#7843,#7844,
#7845,#7846));
#8251=CLOSED_SHELL('',(#7847,#7848,#7849,#7850,#7851,#7852,#7853,#7854,
#7855,#7856));
#8252=CLOSED_SHELL('',(#7857,#7858,#7859,#7860,#7861,#7862,#7863,#7864,
#7865,#7866,#7867,#7868,#7869,#7870,#7871,#7872,#7873,#7874));
#8253=CLOSED_SHELL('',(#7875,#7876,#7877,#7878,#7879,#7880));
#8254=CLOSED_SHELL('',(#7881,#7882,#7883,#7884,#7885,#7886,#7887,#7888,
#7889,#7890));
#8255=CLOSED_SHELL('',(#7891,#7892,#7893,#7894,#7895,#7896,#7897,#7898,
#7899,#7900));
#8256=CLOSED_SHELL('',(#7901,#7902,#7903,#7904,#7905,#7906,#7907));
#8257=CLOSED_SHELL('',(#7908,#7909,#7910,#7911,#7912,#7913,#7914,#7915,
#7916,#7917,#7918,#7919,#7920,#7921,#7922,#7923,#7924,#7925,#7926,#7927,
#7928,#7929,#7930,#7931,#7932,#7933,#7934,#7935,#7936,#7937,#7938,#7939,
#7940,#7941,#7942,#7943,#7944,#7945,#7946,#7947,#7948,#7949,#7950,#7951,
#7952,#7953,#7954));
#8258=CLOSED_SHELL('',(#7955,#7956,#7957,#7958,#7959,#7960,#7961,#7962,
#7963,#7964,#7965,#7966,#7967,#7968));
#8259=CLOSED_SHELL('',(#7969,#7970,#7971,#7972,#7973));
#8260=CLOSED_SHELL('',(#7974,#7975,#7976,#7977,#7978,#7979,#7980,#7981));
#8261=CLOSED_SHELL('',(#7982,#7983,#7984,#7985,#7986,#7987,#7988,#7989));
#8262=CLOSED_SHELL('',(#7990,#7991,#7992,#7993,#7994,#7995,#7996,#7997));
#8263=CLOSED_SHELL('',(#7998,#7999,#8000,#8001,#8002,#8003,#8004,#8005));
#8264=CLOSED_SHELL('',(#8006));
#8265=CLOSED_SHELL('',(#8007));
#8266=CLOSED_SHELL('',(#8008));
#8267=CLOSED_SHELL('',(#8009));
#8268=CLOSED_SHELL('',(#8010));
#8269=CLOSED_SHELL('',(#8011));
#8270=CLOSED_SHELL('',(#8012));
#8271=CLOSED_SHELL('',(#8013));
#8272=CLOSED_SHELL('',(#8014,#8015,#8016,#8017,#8018,#8019,#8020,#8021,
#8022,#8023,#8024,#8025,#8026,#8027,#8028,#8029,#8030,#8031,#8032));
#8273=CLOSED_SHELL('',(#8033,#8034,#8035,#8036));
#8274=CLOSED_SHELL('',(#8037,#8038,#8039,#8040));
#8275=CLOSED_SHELL('',(#8041,#8042,#8043,#8044,#8045,#8046,#8047,#8048,
#8049,#8050,#8051,#8052,#8053,#8054,#8055,#8056,#8057));
#8276=CLOSED_SHELL('',(#8058,#8059,#8060,#8061,#8062,#8063,#8064,#8065));
#8277=CLOSED_SHELL('',(#8066,#8067,#8068,#8069,#8070,#8071,#8072,#8073));
#8278=CLOSED_SHELL('',(#8074,#8075,#8076,#8077,#8078,#8079,#8080,#8081,
#8082,#8083,#8084));
#8279=CLOSED_SHELL('',(#8085,#8086,#8087,#8088,#8089,#8090,#8091,#8092,
#8093,#8094,#8095,#8096,#8097,#8098,#8099,#8100,#8101,#8102));
#8280=CLOSED_SHELL('',(#8103,#8104,#8105,#8106));
#8281=CLOSED_SHELL('',(#8107,#8108,#8109,#8110,#8111,#8112,#8113));
#8282=CLOSED_SHELL('',(#8114,#8115,#8116,#8117,#8118,#8119,#8120,#8121,
#8122,#8123,#8124));
#8283=CLOSED_SHELL('',(#8125,#8126,#8127,#8128));
#8284=CLOSED_SHELL('',(#8129,#8130,#8131,#8132));
#8285=CLOSED_SHELL('',(#8133,#8134,#8135,#8136));
#8286=CLOSED_SHELL('',(#8137,#8138,#8139,#8140));
#8287=CLOSED_SHELL('',(#8141,#8142,#8143,#8144,#8145,#8146,#8147,#8148,
#8149,#8150,#8151));
#8288=CLOSED_SHELL('',(#8152,#8153,#8154,#8155,#8156,#8157,#8158,#8159));
#8289=CLOSED_SHELL('',(#8160,#8161,#8162,#8163,#8164,#8165,#8166,#8167));
#8290=CLOSED_SHELL('',(#8168,#8169,#8170,#8171,#8172,#8173,#8174,#8175,
#8176));
#8291=CLOSED_SHELL('',(#8177,#8178,#8179,#8180,#8181,#8182,#8183,#8184));
#8292=CLOSED_SHELL('',(#8185,#8186,#8187,#8188,#8189,#8190,#8191,#8192));
#8293=CLOSED_SHELL('',(#8193,#8194,#8195,#8196));
#8294=CLOSED_SHELL('',(#8197,#8198,#8199,#8200));
#8295=CLOSED_SHELL('',(#8201,#8202,#8203,#8204,#8205,#8206,#8207,#8208,
#8209,#8210,#8211,#8212,#8213,#8214));
#8296=CLOSED_SHELL('',(#8215,#8216,#8217,#8218,#8219,#8220,#8221,#8222,
#8223,#8224));
#8297=CLOSED_SHELL('',(#8225,#8226,#8227,#8228,#8229));
#8298=CLOSED_SHELL('',(#8230,#8231,#8232));
#8299=CLOSED_SHELL('',(#8233,#8234,#8235,#8236,#8237,#8238,#8239,#8240,
#8241,#8242,#8243,#8244));
#8300=DERIVED_UNIT_ELEMENT(#8384,1.);
#8301=DERIVED_UNIT_ELEMENT(#15214,-3.);
#8302=DERIVED_UNIT_ELEMENT(#8384,1.);
#8303=DERIVED_UNIT_ELEMENT(#15214,-3.);
#8304=DERIVED_UNIT_ELEMENT(#8384,1.);
#8305=DERIVED_UNIT_ELEMENT(#15214,-3.);
#8306=DERIVED_UNIT_ELEMENT(#8384,1.);
#8307=DERIVED_UNIT_ELEMENT(#15214,-3.);
#8308=DERIVED_UNIT_ELEMENT(#8384,1.);
#8309=DERIVED_UNIT_ELEMENT(#15214,-3.);
#8310=DERIVED_UNIT_ELEMENT(#8384,1.);
#8311=DERIVED_UNIT_ELEMENT(#15214,-3.);
#8312=DERIVED_UNIT_ELEMENT(#8384,1.);
#8313=DERIVED_UNIT_ELEMENT(#15214,-3.);
#8314=DERIVED_UNIT_ELEMENT(#8384,1.);
#8315=DERIVED_UNIT_ELEMENT(#15214,-3.);
#8316=DERIVED_UNIT_ELEMENT(#8384,1.);
#8317=DERIVED_UNIT_ELEMENT(#15214,-3.);
#8318=DERIVED_UNIT_ELEMENT(#8384,1.);
#8319=DERIVED_UNIT_ELEMENT(#15214,-3.);
#8320=DERIVED_UNIT_ELEMENT(#8384,1.);
#8321=DERIVED_UNIT_ELEMENT(#15214,-3.);
#8322=DERIVED_UNIT_ELEMENT(#8384,1.);
#8323=DERIVED_UNIT_ELEMENT(#15214,-3.);
#8324=DERIVED_UNIT_ELEMENT(#8384,1.);
#8325=DERIVED_UNIT_ELEMENT(#15214,-3.);
#8326=DERIVED_UNIT_ELEMENT(#8384,1.);
#8327=DERIVED_UNIT_ELEMENT(#15214,-3.);
#8328=DERIVED_UNIT_ELEMENT(#8384,1.);
#8329=DERIVED_UNIT_ELEMENT(#15214,-3.);
#8330=DERIVED_UNIT_ELEMENT(#8384,1.);
#8331=DERIVED_UNIT_ELEMENT(#15214,-3.);
#8332=DERIVED_UNIT_ELEMENT(#8384,1.);
#8333=DERIVED_UNIT_ELEMENT(#15214,-3.);
#8334=DERIVED_UNIT_ELEMENT(#8384,1.);
#8335=DERIVED_UNIT_ELEMENT(#15214,-3.);
#8336=DERIVED_UNIT_ELEMENT(#8384,1.);
#8337=DERIVED_UNIT_ELEMENT(#15214,-3.);
#8338=DERIVED_UNIT_ELEMENT(#8384,1.);
#8339=DERIVED_UNIT_ELEMENT(#15214,-3.);
#8340=DERIVED_UNIT_ELEMENT(#8384,1.);
#8341=DERIVED_UNIT_ELEMENT(#15214,-3.);
#8342=DERIVED_UNIT_ELEMENT(#8384,1.);
#8343=DERIVED_UNIT_ELEMENT(#15214,-3.);
#8344=DERIVED_UNIT_ELEMENT(#8384,1.);
#8345=DERIVED_UNIT_ELEMENT(#15214,-3.);
#8346=DERIVED_UNIT_ELEMENT(#8384,1.);
#8347=DERIVED_UNIT_ELEMENT(#15214,-3.);
#8348=DERIVED_UNIT_ELEMENT(#8384,1.);
#8349=DERIVED_UNIT_ELEMENT(#15214,-3.);
#8350=DERIVED_UNIT_ELEMENT(#8384,1.);
#8351=DERIVED_UNIT_ELEMENT(#15214,-3.);
#8352=DERIVED_UNIT_ELEMENT(#8384,1.);
#8353=DERIVED_UNIT_ELEMENT(#15214,-3.);
#8354=DERIVED_UNIT_ELEMENT(#8384,1.);
#8355=DERIVED_UNIT_ELEMENT(#15214,-3.);
#8356=DERIVED_UNIT_ELEMENT(#8384,1.);
#8357=DERIVED_UNIT_ELEMENT(#15214,-3.);
#8358=DERIVED_UNIT_ELEMENT(#8384,1.);
#8359=DERIVED_UNIT_ELEMENT(#15214,-3.);
#8360=DERIVED_UNIT_ELEMENT(#8384,1.);
#8361=DERIVED_UNIT_ELEMENT(#15214,-3.);
#8362=DERIVED_UNIT_ELEMENT(#8384,1.);
#8363=DERIVED_UNIT_ELEMENT(#15214,-3.);
#8364=DERIVED_UNIT_ELEMENT(#8384,1.);
#8365=DERIVED_UNIT_ELEMENT(#15214,-3.);
#8366=DERIVED_UNIT_ELEMENT(#8384,1.);
#8367=DERIVED_UNIT_ELEMENT(#15214,-3.);
#8368=DERIVED_UNIT_ELEMENT(#8384,1.);
#8369=DERIVED_UNIT_ELEMENT(#15214,-3.);
#8370=DERIVED_UNIT_ELEMENT(#8384,1.);
#8371=DERIVED_UNIT_ELEMENT(#15214,-3.);
#8372=DERIVED_UNIT_ELEMENT(#8384,1.);
#8373=DERIVED_UNIT_ELEMENT(#15214,-3.);
#8374=DERIVED_UNIT_ELEMENT(#8384,1.);
#8375=DERIVED_UNIT_ELEMENT(#15214,-3.);
#8376=DERIVED_UNIT_ELEMENT(#8384,1.);
#8377=DERIVED_UNIT_ELEMENT(#15214,-3.);
#8378=DERIVED_UNIT_ELEMENT(#8384,1.);
#8379=DERIVED_UNIT_ELEMENT(#15214,-3.);
#8380=DERIVED_UNIT_ELEMENT(#8384,1.);
#8381=DERIVED_UNIT_ELEMENT(#15214,-3.);
#8382=DERIVED_UNIT_ELEMENT(#8384,1.);
#8383=DERIVED_UNIT_ELEMENT(#15214,-3.);
#8384=(
MASS_UNIT()
NAMED_UNIT(*)
SI_UNIT(.KILO.,.GRAM.)
);
#8385=DERIVED_UNIT((#8300,#8301));
#8386=DERIVED_UNIT((#8302,#8303));
#8387=DERIVED_UNIT((#8304,#8305));
#8388=DERIVED_UNIT((#8306,#8307));
#8389=DERIVED_UNIT((#8308,#8309));
#8390=DERIVED_UNIT((#8310,#8311));
#8391=DERIVED_UNIT((#8312,#8313));
#8392=DERIVED_UNIT((#8314,#8315));
#8393=DERIVED_UNIT((#8316,#8317));
#8394=DERIVED_UNIT((#8318,#8319));
#8395=DERIVED_UNIT((#8320,#8321));
#8396=DERIVED_UNIT((#8322,#8323));
#8397=DERIVED_UNIT((#8324,#8325));
#8398=DERIVED_UNIT((#8326,#8327));
#8399=DERIVED_UNIT((#8328,#8329));
#8400=DERIVED_UNIT((#8330,#8331));
#8401=DERIVED_UNIT((#8332,#8333));
#8402=DERIVED_UNIT((#8334,#8335));
#8403=DERIVED_UNIT((#8336,#8337));
#8404=DERIVED_UNIT((#8338,#8339));
#8405=DERIVED_UNIT((#8340,#8341));
#8406=DERIVED_UNIT((#8342,#8343));
#8407=DERIVED_UNIT((#8344,#8345));
#8408=DERIVED_UNIT((#8346,#8347));
#8409=DERIVED_UNIT((#8348,#8349));
#8410=DERIVED_UNIT((#8350,#8351));
#8411=DERIVED_UNIT((#8352,#8353));
#8412=DERIVED_UNIT((#8354,#8355));
#8413=DERIVED_UNIT((#8356,#8357));
#8414=DERIVED_UNIT((#8358,#8359));
#8415=DERIVED_UNIT((#8360,#8361));
#8416=DERIVED_UNIT((#8362,#8363));
#8417=DERIVED_UNIT((#8364,#8365));
#8418=DERIVED_UNIT((#8366,#8367));
#8419=DERIVED_UNIT((#8368,#8369));
#8420=DERIVED_UNIT((#8370,#8371));
#8421=DERIVED_UNIT((#8372,#8373));
#8422=DERIVED_UNIT((#8374,#8375));
#8423=DERIVED_UNIT((#8376,#8377));
#8424=DERIVED_UNIT((#8378,#8379));
#8425=DERIVED_UNIT((#8380,#8381));
#8426=DERIVED_UNIT((#8382,#8383));
#8427=MEASURE_REPRESENTATION_ITEM('density measure',
POSITIVE_RATIO_MEASURE(7850.),#8385);
#8428=MEASURE_REPRESENTATION_ITEM('density measure',
POSITIVE_RATIO_MEASURE(7850.),#8386);
#8429=MEASURE_REPRESENTATION_ITEM('density measure',
POSITIVE_RATIO_MEASURE(7850.),#8387);
#8430=MEASURE_REPRESENTATION_ITEM('density measure',
POSITIVE_RATIO_MEASURE(7850.),#8388);
#8431=MEASURE_REPRESENTATION_ITEM('density measure',
POSITIVE_RATIO_MEASURE(7850.),#8389);
#8432=MEASURE_REPRESENTATION_ITEM('density measure',
POSITIVE_RATIO_MEASURE(7850.),#8390);
#8433=MEASURE_REPRESENTATION_ITEM('density measure',
POSITIVE_RATIO_MEASURE(7850.),#8391);
#8434=MEASURE_REPRESENTATION_ITEM('density measure',
POSITIVE_RATIO_MEASURE(7850.),#8392);
#8435=MEASURE_REPRESENTATION_ITEM('density measure',
POSITIVE_RATIO_MEASURE(7850.),#8393);
#8436=MEASURE_REPRESENTATION_ITEM('density measure',
POSITIVE_RATIO_MEASURE(7850.),#8394);
#8437=MEASURE_REPRESENTATION_ITEM('density measure',
POSITIVE_RATIO_MEASURE(7850.),#8395);
#8438=MEASURE_REPRESENTATION_ITEM('density measure',
POSITIVE_RATIO_MEASURE(7850.),#8396);
#8439=MEASURE_REPRESENTATION_ITEM('density measure',
POSITIVE_RATIO_MEASURE(7850.),#8397);
#8440=MEASURE_REPRESENTATION_ITEM('density measure',
POSITIVE_RATIO_MEASURE(7850.),#8398);
#8441=MEASURE_REPRESENTATION_ITEM('density measure',
POSITIVE_RATIO_MEASURE(7850.),#8399);
#8442=MEASURE_REPRESENTATION_ITEM('density measure',
POSITIVE_RATIO_MEASURE(7850.),#8400);
#8443=MEASURE_REPRESENTATION_ITEM('density measure',
POSITIVE_RATIO_MEASURE(7850.),#8401);
#8444=MEASURE_REPRESENTATION_ITEM('density measure',
POSITIVE_RATIO_MEASURE(7850.),#8402);
#8445=MEASURE_REPRESENTATION_ITEM('density measure',
POSITIVE_RATIO_MEASURE(7850.),#8403);
#8446=MEASURE_REPRESENTATION_ITEM('density measure',
POSITIVE_RATIO_MEASURE(7850.),#8404);
#8447=MEASURE_REPRESENTATION_ITEM('density measure',
POSITIVE_RATIO_MEASURE(7850.),#8405);
#8448=MEASURE_REPRESENTATION_ITEM('density measure',
POSITIVE_RATIO_MEASURE(7850.),#8406);
#8449=MEASURE_REPRESENTATION_ITEM('density measure',
POSITIVE_RATIO_MEASURE(7850.),#8407);
#8450=MEASURE_REPRESENTATION_ITEM('density measure',
POSITIVE_RATIO_MEASURE(7850.),#8408);
#8451=MEASURE_REPRESENTATION_ITEM('density measure',
POSITIVE_RATIO_MEASURE(7850.),#8409);
#8452=MEASURE_REPRESENTATION_ITEM('density measure',
POSITIVE_RATIO_MEASURE(7850.),#8410);
#8453=MEASURE_REPRESENTATION_ITEM('density measure',
POSITIVE_RATIO_MEASURE(7850.),#8411);
#8454=MEASURE_REPRESENTATION_ITEM('density measure',
POSITIVE_RATIO_MEASURE(7850.),#8412);
#8455=MEASURE_REPRESENTATION_ITEM('density measure',
POSITIVE_RATIO_MEASURE(7850.),#8413);
#8456=MEASURE_REPRESENTATION_ITEM('density measure',
POSITIVE_RATIO_MEASURE(7850.),#8414);
#8457=MEASURE_REPRESENTATION_ITEM('density measure',
POSITIVE_RATIO_MEASURE(7850.),#8415);
#8458=MEASURE_REPRESENTATION_ITEM('density measure',
POSITIVE_RATIO_MEASURE(7850.),#8416);
#8459=MEASURE_REPRESENTATION_ITEM('density measure',
POSITIVE_RATIO_MEASURE(7850.),#8417);
#8460=MEASURE_REPRESENTATION_ITEM('density measure',
POSITIVE_RATIO_MEASURE(7850.),#8418);
#8461=MEASURE_REPRESENTATION_ITEM('density measure',
POSITIVE_RATIO_MEASURE(7850.),#8419);
#8462=MEASURE_REPRESENTATION_ITEM('density measure',
POSITIVE_RATIO_MEASURE(7850.),#8420);
#8463=MEASURE_REPRESENTATION_ITEM('density measure',
POSITIVE_RATIO_MEASURE(7850.),#8421);
#8464=MEASURE_REPRESENTATION_ITEM('density measure',
POSITIVE_RATIO_MEASURE(7850.),#8422);
#8465=MEASURE_REPRESENTATION_ITEM('density measure',
POSITIVE_RATIO_MEASURE(7850.),#8423);
#8466=MEASURE_REPRESENTATION_ITEM('density measure',
POSITIVE_RATIO_MEASURE(7850.),#8424);
#8467=MEASURE_REPRESENTATION_ITEM('density measure',
POSITIVE_RATIO_MEASURE(7850.),#8425);
#8468=MEASURE_REPRESENTATION_ITEM('density measure',
POSITIVE_RATIO_MEASURE(7850.),#8426);
#8469=PROPERTY_DEFINITION_REPRESENTATION(#8679,#8553);
#8470=PROPERTY_DEFINITION_REPRESENTATION(#8680,#8554);
#8471=PROPERTY_DEFINITION_REPRESENTATION(#8681,#8555);
#8472=PROPERTY_DEFINITION_REPRESENTATION(#8682,#8556);
#8473=PROPERTY_DEFINITION_REPRESENTATION(#8683,#8557);
#8474=PROPERTY_DEFINITION_REPRESENTATION(#8684,#8558);
#8475=PROPERTY_DEFINITION_REPRESENTATION(#8685,#8559);
#8476=PROPERTY_DEFINITION_REPRESENTATION(#8686,#8560);
#8477=PROPERTY_DEFINITION_REPRESENTATION(#8687,#8561);
#8478=PROPERTY_DEFINITION_REPRESENTATION(#8688,#8562);
#8479=PROPERTY_DEFINITION_REPRESENTATION(#8689,#8563);
#8480=PROPERTY_DEFINITION_REPRESENTATION(#8690,#8564);
#8481=PROPERTY_DEFINITION_REPRESENTATION(#8691,#8565);
#8482=PROPERTY_DEFINITION_REPRESENTATION(#8692,#8566);
#8483=PROPERTY_DEFINITION_REPRESENTATION(#8693,#8567);
#8484=PROPERTY_DEFINITION_REPRESENTATION(#8694,#8568);
#8485=PROPERTY_DEFINITION_REPRESENTATION(#8695,#8569);
#8486=PROPERTY_DEFINITION_REPRESENTATION(#8696,#8570);
#8487=PROPERTY_DEFINITION_REPRESENTATION(#8697,#8571);
#8488=PROPERTY_DEFINITION_REPRESENTATION(#8698,#8572);
#8489=PROPERTY_DEFINITION_REPRESENTATION(#8699,#8573);
#8490=PROPERTY_DEFINITION_REPRESENTATION(#8700,#8574);
#8491=PROPERTY_DEFINITION_REPRESENTATION(#8701,#8575);
#8492=PROPERTY_DEFINITION_REPRESENTATION(#8702,#8576);
#8493=PROPERTY_DEFINITION_REPRESENTATION(#8703,#8577);
#8494=PROPERTY_DEFINITION_REPRESENTATION(#8704,#8578);
#8495=PROPERTY_DEFINITION_REPRESENTATION(#8705,#8579);
#8496=PROPERTY_DEFINITION_REPRESENTATION(#8706,#8580);
#8497=PROPERTY_DEFINITION_REPRESENTATION(#8707,#8581);
#8498=PROPERTY_DEFINITION_REPRESENTATION(#8708,#8582);
#8499=PROPERTY_DEFINITION_REPRESENTATION(#8709,#8583);
#8500=PROPERTY_DEFINITION_REPRESENTATION(#8710,#8584);
#8501=PROPERTY_DEFINITION_REPRESENTATION(#8711,#8585);
#8502=PROPERTY_DEFINITION_REPRESENTATION(#8712,#8586);
#8503=PROPERTY_DEFINITION_REPRESENTATION(#8713,#8587);
#8504=PROPERTY_DEFINITION_REPRESENTATION(#8714,#8588);
#8505=PROPERTY_DEFINITION_REPRESENTATION(#8715,#8589);
#8506=PROPERTY_DEFINITION_REPRESENTATION(#8716,#8590);
#8507=PROPERTY_DEFINITION_REPRESENTATION(#8717,#8591);
#8508=PROPERTY_DEFINITION_REPRESENTATION(#8718,#8592);
#8509=PROPERTY_DEFINITION_REPRESENTATION(#8719,#8593);
#8510=PROPERTY_DEFINITION_REPRESENTATION(#8720,#8594);
#8511=PROPERTY_DEFINITION_REPRESENTATION(#8721,#8595);
#8512=PROPERTY_DEFINITION_REPRESENTATION(#8722,#8596);
#8513=PROPERTY_DEFINITION_REPRESENTATION(#8723,#8597);
#8514=PROPERTY_DEFINITION_REPRESENTATION(#8724,#8598);
#8515=PROPERTY_DEFINITION_REPRESENTATION(#8725,#8599);
#8516=PROPERTY_DEFINITION_REPRESENTATION(#8726,#8600);
#8517=PROPERTY_DEFINITION_REPRESENTATION(#8727,#8601);
#8518=PROPERTY_DEFINITION_REPRESENTATION(#8728,#8602);
#8519=PROPERTY_DEFINITION_REPRESENTATION(#8729,#8603);
#8520=PROPERTY_DEFINITION_REPRESENTATION(#8730,#8604);
#8521=PROPERTY_DEFINITION_REPRESENTATION(#8731,#8605);
#8522=PROPERTY_DEFINITION_REPRESENTATION(#8732,#8606);
#8523=PROPERTY_DEFINITION_REPRESENTATION(#8733,#8607);
#8524=PROPERTY_DEFINITION_REPRESENTATION(#8734,#8608);
#8525=PROPERTY_DEFINITION_REPRESENTATION(#8735,#8609);
#8526=PROPERTY_DEFINITION_REPRESENTATION(#8736,#8610);
#8527=PROPERTY_DEFINITION_REPRESENTATION(#8737,#8611);
#8528=PROPERTY_DEFINITION_REPRESENTATION(#8738,#8612);
#8529=PROPERTY_DEFINITION_REPRESENTATION(#8739,#8613);
#8530=PROPERTY_DEFINITION_REPRESENTATION(#8740,#8614);
#8531=PROPERTY_DEFINITION_REPRESENTATION(#8741,#8615);
#8532=PROPERTY_DEFINITION_REPRESENTATION(#8742,#8616);
#8533=PROPERTY_DEFINITION_REPRESENTATION(#8743,#8617);
#8534=PROPERTY_DEFINITION_REPRESENTATION(#8744,#8618);
#8535=PROPERTY_DEFINITION_REPRESENTATION(#8745,#8619);
#8536=PROPERTY_DEFINITION_REPRESENTATION(#8746,#8620);
#8537=PROPERTY_DEFINITION_REPRESENTATION(#8747,#8621);
#8538=PROPERTY_DEFINITION_REPRESENTATION(#8748,#8622);
#8539=PROPERTY_DEFINITION_REPRESENTATION(#8749,#8623);
#8540=PROPERTY_DEFINITION_REPRESENTATION(#8750,#8624);
#8541=PROPERTY_DEFINITION_REPRESENTATION(#8751,#8625);
#8542=PROPERTY_DEFINITION_REPRESENTATION(#8752,#8626);
#8543=PROPERTY_DEFINITION_REPRESENTATION(#8753,#8627);
#8544=PROPERTY_DEFINITION_REPRESENTATION(#8754,#8628);
#8545=PROPERTY_DEFINITION_REPRESENTATION(#8755,#8629);
#8546=PROPERTY_DEFINITION_REPRESENTATION(#8756,#8630);
#8547=PROPERTY_DEFINITION_REPRESENTATION(#8757,#8631);
#8548=PROPERTY_DEFINITION_REPRESENTATION(#8758,#8632);
#8549=PROPERTY_DEFINITION_REPRESENTATION(#8759,#8633);
#8550=PROPERTY_DEFINITION_REPRESENTATION(#8760,#8634);
#8551=PROPERTY_DEFINITION_REPRESENTATION(#8761,#8635);
#8552=PROPERTY_DEFINITION_REPRESENTATION(#8762,#8636);
#8553=REPRESENTATION('material name',(#8637),#15165);
#8554=REPRESENTATION('density',(#8427),#15165);
#8555=REPRESENTATION('material name',(#8638),#15166);
#8556=REPRESENTATION('density',(#8428),#15166);
#8557=REPRESENTATION('material name',(#8639),#15167);
#8558=REPRESENTATION('density',(#8429),#15167);
#8559=REPRESENTATION('material name',(#8640),#15168);
#8560=REPRESENTATION('density',(#8430),#15168);
#8561=REPRESENTATION('material name',(#8641),#15169);
#8562=REPRESENTATION('density',(#8431),#15169);
#8563=REPRESENTATION('material name',(#8642),#15170);
#8564=REPRESENTATION('density',(#8432),#15170);
#8565=REPRESENTATION('material name',(#8643),#15171);
#8566=REPRESENTATION('density',(#8433),#15171);
#8567=REPRESENTATION('material name',(#8644),#15172);
#8568=REPRESENTATION('density',(#8434),#15172);
#8569=REPRESENTATION('material name',(#8645),#15173);
#8570=REPRESENTATION('density',(#8435),#15173);
#8571=REPRESENTATION('material name',(#8646),#15174);
#8572=REPRESENTATION('density',(#8436),#15174);
#8573=REPRESENTATION('material name',(#8647),#15175);
#8574=REPRESENTATION('density',(#8437),#15175);
#8575=REPRESENTATION('material name',(#8648),#15176);
#8576=REPRESENTATION('density',(#8438),#15176);
#8577=REPRESENTATION('material name',(#8649),#15177);
#8578=REPRESENTATION('density',(#8439),#15177);
#8579=REPRESENTATION('material name',(#8650),#15178);
#8580=REPRESENTATION('density',(#8440),#15178);
#8581=REPRESENTATION('material name',(#8651),#15179);
#8582=REPRESENTATION('density',(#8441),#15179);
#8583=REPRESENTATION('material name',(#8652),#15180);
#8584=REPRESENTATION('density',(#8442),#15180);
#8585=REPRESENTATION('material name',(#8653),#15182);
#8586=REPRESENTATION('density',(#8443),#15182);
#8587=REPRESENTATION('material name',(#8654),#15183);
#8588=REPRESENTATION('density',(#8444),#15183);
#8589=REPRESENTATION('material name',(#8655),#15184);
#8590=REPRESENTATION('density',(#8445),#15184);
#8591=REPRESENTATION('material name',(#8656),#15185);
#8592=REPRESENTATION('density',(#8446),#15185);
#8593=REPRESENTATION('material name',(#8657),#15186);
#8594=REPRESENTATION('density',(#8447),#15186);
#8595=REPRESENTATION('material name',(#8658),#15188);
#8596=REPRESENTATION('density',(#8448),#15188);
#8597=REPRESENTATION('material name',(#8659),#15189);
#8598=REPRESENTATION('density',(#8449),#15189);
#8599=REPRESENTATION('material name',(#8660),#15190);
#8600=REPRESENTATION('density',(#8450),#15190);
#8601=REPRESENTATION('material name',(#8661),#15192);
#8602=REPRESENTATION('density',(#8451),#15192);
#8603=REPRESENTATION('material name',(#8662),#15193);
#8604=REPRESENTATION('density',(#8452),#15193);
#8605=REPRESENTATION('material name',(#8663),#15194);
#8606=REPRESENTATION('density',(#8453),#15194);
#8607=REPRESENTATION('material name',(#8664),#15195);
#8608=REPRESENTATION('density',(#8454),#15195);
#8609=REPRESENTATION('material name',(#8665),#15196);
#8610=REPRESENTATION('density',(#8455),#15196);
#8611=REPRESENTATION('material name',(#8666),#15197);
#8612=REPRESENTATION('density',(#8456),#15197);
#8613=REPRESENTATION('material name',(#8667),#15198);
#8614=REPRESENTATION('density',(#8457),#15198);
#8615=REPRESENTATION('material name',(#8668),#15199);
#8616=REPRESENTATION('density',(#8458),#15199);
#8617=REPRESENTATION('material name',(#8669),#15200);
#8618=REPRESENTATION('density',(#8459),#15200);
#8619=REPRESENTATION('material name',(#8670),#15201);
#8620=REPRESENTATION('density',(#8460),#15201);
#8621=REPRESENTATION('material name',(#8671),#15202);
#8622=REPRESENTATION('density',(#8461),#15202);
#8623=REPRESENTATION('material name',(#8672),#15204);
#8624=REPRESENTATION('density',(#8462),#15204);
#8625=REPRESENTATION('material name',(#8673),#15205);
#8626=REPRESENTATION('density',(#8463),#15205);
#8627=REPRESENTATION('material name',(#8674),#15206);
#8628=REPRESENTATION('density',(#8464),#15206);
#8629=REPRESENTATION('material name',(#8675),#15208);
#8630=REPRESENTATION('density',(#8465),#15208);
#8631=REPRESENTATION('material name',(#8676),#15209);
#8632=REPRESENTATION('density',(#8466),#15209);
#8633=REPRESENTATION('material name',(#8677),#15210);
#8634=REPRESENTATION('density',(#8467),#15210);
#8635=REPRESENTATION('material name',(#8678),#15211);
#8636=REPRESENTATION('density',(#8468),#15211);
#8637=DESCRIPTIVE_REPRESENTATION_ITEM('Steel','Steel');
#8638=DESCRIPTIVE_REPRESENTATION_ITEM('Steel','Steel');
#8639=DESCRIPTIVE_REPRESENTATION_ITEM('Steel','Steel');
#8640=DESCRIPTIVE_REPRESENTATION_ITEM('Steel','Steel');
#8641=DESCRIPTIVE_REPRESENTATION_ITEM('Steel','Steel');
#8642=DESCRIPTIVE_REPRESENTATION_ITEM('Steel','Steel');
#8643=DESCRIPTIVE_REPRESENTATION_ITEM('Steel','Steel');
#8644=DESCRIPTIVE_REPRESENTATION_ITEM('Steel','Steel');
#8645=DESCRIPTIVE_REPRESENTATION_ITEM('Steel','Steel');
#8646=DESCRIPTIVE_REPRESENTATION_ITEM('Steel','Steel');
#8647=DESCRIPTIVE_REPRESENTATION_ITEM('Steel','Steel');
#8648=DESCRIPTIVE_REPRESENTATION_ITEM('Steel','Steel');
#8649=DESCRIPTIVE_REPRESENTATION_ITEM('Steel','Steel');
#8650=DESCRIPTIVE_REPRESENTATION_ITEM('Steel','Steel');
#8651=DESCRIPTIVE_REPRESENTATION_ITEM('Steel','Steel');
#8652=DESCRIPTIVE_REPRESENTATION_ITEM('Steel','Steel');
#8653=DESCRIPTIVE_REPRESENTATION_ITEM('Steel','Steel');
#8654=DESCRIPTIVE_REPRESENTATION_ITEM('Steel','Steel');
#8655=DESCRIPTIVE_REPRESENTATION_ITEM('Steel','Steel');
#8656=DESCRIPTIVE_REPRESENTATION_ITEM('Steel','Steel');
#8657=DESCRIPTIVE_REPRESENTATION_ITEM('Steel','Steel');
#8658=DESCRIPTIVE_REPRESENTATION_ITEM('Steel','Steel');
#8659=DESCRIPTIVE_REPRESENTATION_ITEM('Steel','Steel');
#8660=DESCRIPTIVE_REPRESENTATION_ITEM('Steel','Steel');
#8661=DESCRIPTIVE_REPRESENTATION_ITEM('Steel','Steel');
#8662=DESCRIPTIVE_REPRESENTATION_ITEM('Steel','Steel');
#8663=DESCRIPTIVE_REPRESENTATION_ITEM('Steel','Steel');
#8664=DESCRIPTIVE_REPRESENTATION_ITEM('Steel','Steel');
#8665=DESCRIPTIVE_REPRESENTATION_ITEM('Steel','Steel');
#8666=DESCRIPTIVE_REPRESENTATION_ITEM('Steel','Steel');
#8667=DESCRIPTIVE_REPRESENTATION_ITEM('Steel','Steel');
#8668=DESCRIPTIVE_REPRESENTATION_ITEM('Steel','Steel');
#8669=DESCRIPTIVE_REPRESENTATION_ITEM('Steel','Steel');
#8670=DESCRIPTIVE_REPRESENTATION_ITEM('Steel','Steel');
#8671=DESCRIPTIVE_REPRESENTATION_ITEM('Steel','Steel');
#8672=DESCRIPTIVE_REPRESENTATION_ITEM('Steel','Steel');
#8673=DESCRIPTIVE_REPRESENTATION_ITEM('Steel','Steel');
#8674=DESCRIPTIVE_REPRESENTATION_ITEM('Steel','Steel');
#8675=DESCRIPTIVE_REPRESENTATION_ITEM('Steel','Steel');
#8676=DESCRIPTIVE_REPRESENTATION_ITEM('Steel','Steel');
#8677=DESCRIPTIVE_REPRESENTATION_ITEM('Steel','Steel');
#8678=DESCRIPTIVE_REPRESENTATION_ITEM('Steel','Steel');
#8679=PROPERTY_DEFINITION('material property','material name',#15453);
#8680=PROPERTY_DEFINITION('material property','density of part',#15453);
#8681=PROPERTY_DEFINITION('material property','material name',#15454);
#8682=PROPERTY_DEFINITION('material property','density of part',#15454);
#8683=PROPERTY_DEFINITION('material property','material name',#15455);
#8684=PROPERTY_DEFINITION('material property','density of part',#15455);
#8685=PROPERTY_DEFINITION('material property','material name',#15456);
#8686=PROPERTY_DEFINITION('material property','density of part',#15456);
#8687=PROPERTY_DEFINITION('material property','material name',#15457);
#8688=PROPERTY_DEFINITION('material property','density of part',#15457);
#8689=PROPERTY_DEFINITION('material property','material name',#15458);
#8690=PROPERTY_DEFINITION('material property','density of part',#15458);
#8691=PROPERTY_DEFINITION('material property','material name',#15459);
#8692=PROPERTY_DEFINITION('material property','density of part',#15459);
#8693=PROPERTY_DEFINITION('material property','material name',#15460);
#8694=PROPERTY_DEFINITION('material property','density of part',#15460);
#8695=PROPERTY_DEFINITION('material property','material name',#15461);
#8696=PROPERTY_DEFINITION('material property','density of part',#15461);
#8697=PROPERTY_DEFINITION('material property','material name',#15462);
#8698=PROPERTY_DEFINITION('material property','density of part',#15462);
#8699=PROPERTY_DEFINITION('material property','material name',#15463);
#8700=PROPERTY_DEFINITION('material property','density of part',#15463);
#8701=PROPERTY_DEFINITION('material property','material name',#15464);
#8702=PROPERTY_DEFINITION('material property','density of part',#15464);
#8703=PROPERTY_DEFINITION('material property','material name',#15465);
#8704=PROPERTY_DEFINITION('material property','density of part',#15465);
#8705=PROPERTY_DEFINITION('material property','material name',#15466);
#8706=PROPERTY_DEFINITION('material property','density of part',#15466);
#8707=PROPERTY_DEFINITION('material property','material name',#15467);
#8708=PROPERTY_DEFINITION('material property','density of part',#15467);
#8709=PROPERTY_DEFINITION('material property','material name',#15468);
#8710=PROPERTY_DEFINITION('material property','density of part',#15468);
#8711=PROPERTY_DEFINITION('material property','material name',#15470);
#8712=PROPERTY_DEFINITION('material property','density of part',#15470);
#8713=PROPERTY_DEFINITION('material property','material name',#15471);
#8714=PROPERTY_DEFINITION('material property','density of part',#15471);
#8715=PROPERTY_DEFINITION('material property','material name',#15472);
#8716=PROPERTY_DEFINITION('material property','density of part',#15472);
#8717=PROPERTY_DEFINITION('material property','material name',#15473);
#8718=PROPERTY_DEFINITION('material property','density of part',#15473);
#8719=PROPERTY_DEFINITION('material property','material name',#15474);
#8720=PROPERTY_DEFINITION('material property','density of part',#15474);
#8721=PROPERTY_DEFINITION('material property','material name',#15476);
#8722=PROPERTY_DEFINITION('material property','density of part',#15476);
#8723=PROPERTY_DEFINITION('material property','material name',#15477);
#8724=PROPERTY_DEFINITION('material property','density of part',#15477);
#8725=PROPERTY_DEFINITION('material property','material name',#15478);
#8726=PROPERTY_DEFINITION('material property','density of part',#15478);
#8727=PROPERTY_DEFINITION('material property','material name',#15480);
#8728=PROPERTY_DEFINITION('material property','density of part',#15480);
#8729=PROPERTY_DEFINITION('material property','material name',#15481);
#8730=PROPERTY_DEFINITION('material property','density of part',#15481);
#8731=PROPERTY_DEFINITION('material property','material name',#15482);
#8732=PROPERTY_DEFINITION('material property','density of part',#15482);
#8733=PROPERTY_DEFINITION('material property','material name',#15483);
#8734=PROPERTY_DEFINITION('material property','density of part',#15483);
#8735=PROPERTY_DEFINITION('material property','material name',#15484);
#8736=PROPERTY_DEFINITION('material property','density of part',#15484);
#8737=PROPERTY_DEFINITION('material property','material name',#15485);
#8738=PROPERTY_DEFINITION('material property','density of part',#15485);
#8739=PROPERTY_DEFINITION('material property','material name',#15486);
#8740=PROPERTY_DEFINITION('material property','density of part',#15486);
#8741=PROPERTY_DEFINITION('material property','material name',#15487);
#8742=PROPERTY_DEFINITION('material property','density of part',#15487);
#8743=PROPERTY_DEFINITION('material property','material name',#15488);
#8744=PROPERTY_DEFINITION('material property','density of part',#15488);
#8745=PROPERTY_DEFINITION('material property','material name',#15489);
#8746=PROPERTY_DEFINITION('material property','density of part',#15489);
#8747=PROPERTY_DEFINITION('material property','material name',#15490);
#8748=PROPERTY_DEFINITION('material property','density of part',#15490);
#8749=PROPERTY_DEFINITION('material property','material name',#15492);
#8750=PROPERTY_DEFINITION('material property','density of part',#15492);
#8751=PROPERTY_DEFINITION('material property','material name',#15493);
#8752=PROPERTY_DEFINITION('material property','density of part',#15493);
#8753=PROPERTY_DEFINITION('material property','material name',#15494);
#8754=PROPERTY_DEFINITION('material property','density of part',#15494);
#8755=PROPERTY_DEFINITION('material property','material name',#15496);
#8756=PROPERTY_DEFINITION('material property','density of part',#15496);
#8757=PROPERTY_DEFINITION('material property','material name',#15497);
#8758=PROPERTY_DEFINITION('material property','density of part',#15497);
#8759=PROPERTY_DEFINITION('material property','material name',#15498);
#8760=PROPERTY_DEFINITION('material property','density of part',#15498);
#8761=PROPERTY_DEFINITION('material property','material name',#15499);
#8762=PROPERTY_DEFINITION('material property','density of part',#15499);
#8763=AXIS2_PLACEMENT_3D('',#12366,#9754,#9755);
#8764=AXIS2_PLACEMENT_3D('',#12367,#9756,#9757);
#8765=AXIS2_PLACEMENT_3D('',#12368,#9758,#9759);
#8766=AXIS2_PLACEMENT_3D('',#12369,#9760,#9761);
#8767=AXIS2_PLACEMENT_3D('',#12371,#9762,#9763);
#8768=AXIS2_PLACEMENT_3D('',#12374,#9765,#9766);
#8769=AXIS2_PLACEMENT_3D('',#12375,#9767,#9768);
#8770=AXIS2_PLACEMENT_3D('',#12377,#9769,#9770);
#8771=AXIS2_PLACEMENT_3D('',#12380,#9772,#9773);
#8772=AXIS2_PLACEMENT_3D('',#12381,#9774,#9775);
#8773=AXIS2_PLACEMENT_3D('',#12383,#9776,#9777);
#8774=AXIS2_PLACEMENT_3D('',#12386,#9779,#9780);
#8775=AXIS2_PLACEMENT_3D('',#12387,#9781,#9782);
#8776=AXIS2_PLACEMENT_3D('',#12389,#9783,#9784);
#8777=AXIS2_PLACEMENT_3D('',#12392,#9786,#9787);
#8778=AXIS2_PLACEMENT_3D('',#12393,#9788,#9789);
#8779=AXIS2_PLACEMENT_3D('',#12395,#9790,#9791);
#8780=AXIS2_PLACEMENT_3D('',#12398,#9793,#9794);
#8781=AXIS2_PLACEMENT_3D('',#12399,#9795,#9796);
#8782=AXIS2_PLACEMENT_3D('',#12401,#9797,#9798);
#8783=AXIS2_PLACEMENT_3D('',#12404,#9800,#9801);
#8784=AXIS2_PLACEMENT_3D('',#12405,#9802,#9803);
#8785=AXIS2_PLACEMENT_3D('',#12407,#9804,#9805);
#8786=AXIS2_PLACEMENT_3D('',#12410,#9807,#9808);
#8787=AXIS2_PLACEMENT_3D('',#12411,#9809,#9810);
#8788=AXIS2_PLACEMENT_3D('',#12413,#9811,#9812);
#8789=AXIS2_PLACEMENT_3D('',#12416,#9814,#9815);
#8790=AXIS2_PLACEMENT_3D('',#12417,#9816,#9817);
#8791=AXIS2_PLACEMENT_3D('',#12419,#9818,#9819);
#8792=AXIS2_PLACEMENT_3D('',#12422,#9821,#9822);
#8793=AXIS2_PLACEMENT_3D('',#12423,#9823,#9824);
#8794=AXIS2_PLACEMENT_3D('',#12425,#9825,#9826);
#8795=AXIS2_PLACEMENT_3D('',#12428,#9828,#9829);
#8796=AXIS2_PLACEMENT_3D('',#12429,#9830,#9831);
#8797=AXIS2_PLACEMENT_3D('',#12431,#9832,#9833);
#8798=AXIS2_PLACEMENT_3D('',#12434,#9835,#9836);
#8799=AXIS2_PLACEMENT_3D('',#12435,#9837,#9838);
#8800=AXIS2_PLACEMENT_3D('',#12437,#9839,#9840);
#8801=AXIS2_PLACEMENT_3D('',#12440,#9842,#9843);
#8802=AXIS2_PLACEMENT_3D('',#12441,#9844,#9845);
#8803=AXIS2_PLACEMENT_3D('',#12450,#9850,#9851);
#8804=AXIS2_PLACEMENT_3D('',#12456,#9855,#9856);
#8805=AXIS2_PLACEMENT_3D('',#12462,#9860,#9861);
#8806=AXIS2_PLACEMENT_3D('',#12465,#9864,#9865);
#8807=AXIS2_PLACEMENT_3D('',#12466,#9866,#9867);
#8808=AXIS2_PLACEMENT_3D('',#12467,#9868,#9869);
#8809=AXIS2_PLACEMENT_3D('',#12468,#9870,#9871);
#8810=AXIS2_PLACEMENT_3D('',#12470,#9872,#9873);
#8811=AXIS2_PLACEMENT_3D('',#12473,#9875,#9876);
#8812=AXIS2_PLACEMENT_3D('',#12474,#9877,#9878);
#8813=AXIS2_PLACEMENT_3D('',#12476,#9879,#9880);
#8814=AXIS2_PLACEMENT_3D('',#12479,#9882,#9883);
#8815=AXIS2_PLACEMENT_3D('',#12480,#9884,#9885);
#8816=AXIS2_PLACEMENT_3D('',#12482,#9886,#9887);
#8817=AXIS2_PLACEMENT_3D('',#12485,#9889,#9890);
#8818=AXIS2_PLACEMENT_3D('',#12486,#9891,#9892);
#8819=AXIS2_PLACEMENT_3D('',#12488,#9893,#9894);
#8820=AXIS2_PLACEMENT_3D('',#12491,#9896,#9897);
#8821=AXIS2_PLACEMENT_3D('',#12492,#9898,#9899);
#8822=AXIS2_PLACEMENT_3D('',#12501,#9904,#9905);
#8823=AXIS2_PLACEMENT_3D('',#12507,#9909,#9910);
#8824=AXIS2_PLACEMENT_3D('',#12513,#9914,#9915);
#8825=AXIS2_PLACEMENT_3D('',#12516,#9918,#9919);
#8826=AXIS2_PLACEMENT_3D('',#12517,#9920,#9921);
#8827=AXIS2_PLACEMENT_3D('',#12518,#9922,#9923);
#8828=AXIS2_PLACEMENT_3D('',#12519,#9924,#9925);
#8829=AXIS2_PLACEMENT_3D('',#12528,#9930,#9931);
#8830=AXIS2_PLACEMENT_3D('',#12534,#9935,#9936);
#8831=AXIS2_PLACEMENT_3D('',#12540,#9940,#9941);
#8832=AXIS2_PLACEMENT_3D('',#12543,#9944,#9945);
#8833=AXIS2_PLACEMENT_3D('',#12544,#9946,#9947);
#8834=AXIS2_PLACEMENT_3D('',#12545,#9948,#9949);
#8835=AXIS2_PLACEMENT_3D('',#12546,#9950,#9951);
#8836=AXIS2_PLACEMENT_3D('',#12555,#9956,#9957);
#8837=AXIS2_PLACEMENT_3D('',#12561,#9961,#9962);
#8838=AXIS2_PLACEMENT_3D('',#12567,#9966,#9967);
#8839=AXIS2_PLACEMENT_3D('',#12570,#9970,#9971);
#8840=AXIS2_PLACEMENT_3D('',#12571,#9972,#9973);
#8841=AXIS2_PLACEMENT_3D('',#12572,#9974,#9975);
#8842=AXIS2_PLACEMENT_3D('',#12573,#9976,#9977);
#8843=AXIS2_PLACEMENT_3D('',#12575,#9978,#9979);
#8844=AXIS2_PLACEMENT_3D('',#12578,#9981,#9982);
#8845=AXIS2_PLACEMENT_3D('',#12579,#9983,#9984);
#8846=AXIS2_PLACEMENT_3D('',#12581,#9985,#9986);
#8847=AXIS2_PLACEMENT_3D('',#12584,#9988,#9989);
#8848=AXIS2_PLACEMENT_3D('',#12585,#9990,#9991);
#8849=AXIS2_PLACEMENT_3D('',#12586,#9992,#9993);
#8850=AXIS2_PLACEMENT_3D('',#12588,#9994,#9995);
#8851=AXIS2_PLACEMENT_3D('',#12591,#9997,#9998);
#8852=AXIS2_PLACEMENT_3D('',#12592,#9999,#10000);
#8853=AXIS2_PLACEMENT_3D('',#12593,#10001,#10002);
#8854=AXIS2_PLACEMENT_3D('',#12595,#10003,#10004);
#8855=AXIS2_PLACEMENT_3D('',#12598,#10006,#10007);
#8856=AXIS2_PLACEMENT_3D('',#12599,#10008,#10009);
#8857=AXIS2_PLACEMENT_3D('',#12600,#10010,#10011);
#8858=AXIS2_PLACEMENT_3D('',#12602,#10012,#10013);
#8859=AXIS2_PLACEMENT_3D('',#12605,#10015,#10016);
#8860=AXIS2_PLACEMENT_3D('',#12606,#10017,#10018);
#8861=AXIS2_PLACEMENT_3D('',#12607,#10019,#10020);
#8862=AXIS2_PLACEMENT_3D('',#12609,#10021,#10022);
#8863=AXIS2_PLACEMENT_3D('',#12612,#10024,#10025);
#8864=AXIS2_PLACEMENT_3D('',#12613,#10026,#10027);
#8865=AXIS2_PLACEMENT_3D('',#12615,#10028,#10029);
#8866=AXIS2_PLACEMENT_3D('',#12618,#10031,#10032);
#8867=AXIS2_PLACEMENT_3D('',#12619,#10033,#10034);
#8868=AXIS2_PLACEMENT_3D('',#12621,#10035,#10036);
#8869=AXIS2_PLACEMENT_3D('',#12624,#10038,#10039);
#8870=AXIS2_PLACEMENT_3D('',#12625,#10040,#10041);
#8871=AXIS2_PLACEMENT_3D('',#12627,#10042,#10043);
#8872=AXIS2_PLACEMENT_3D('',#12630,#10045,#10046);
#8873=AXIS2_PLACEMENT_3D('',#12631,#10047,#10048);
#8874=AXIS2_PLACEMENT_3D('',#12633,#10049,#10050);
#8875=AXIS2_PLACEMENT_3D('',#12636,#10052,#10053);
#8876=AXIS2_PLACEMENT_3D('',#12637,#10054,#10055);
#8877=AXIS2_PLACEMENT_3D('',#12639,#10056,#10057);
#8878=AXIS2_PLACEMENT_3D('',#12642,#10059,#10060);
#8879=AXIS2_PLACEMENT_3D('',#12643,#10061,#10062);
#8880=AXIS2_PLACEMENT_3D('',#12645,#10063,#10064);
#8881=AXIS2_PLACEMENT_3D('',#12648,#10066,#10067);
#8882=AXIS2_PLACEMENT_3D('',#12649,#10068,#10069);
#8883=AXIS2_PLACEMENT_3D('',#12651,#10070,#10071);
#8884=AXIS2_PLACEMENT_3D('',#12654,#10073,#10074);
#8885=AXIS2_PLACEMENT_3D('',#12655,#10075,#10076);
#8886=AXIS2_PLACEMENT_3D('',#12657,#10077,#10078);
#8887=AXIS2_PLACEMENT_3D('',#12660,#10080,#10081);
#8888=AXIS2_PLACEMENT_3D('',#12661,#10082,#10083);
#8889=AXIS2_PLACEMENT_3D('',#12663,#10084,#10085);
#8890=AXIS2_PLACEMENT_3D('',#12664,#10086,#10087);
#8891=AXIS2_PLACEMENT_3D('',#12666,#10088,#10089);
#8892=AXIS2_PLACEMENT_3D('',#12668,#10091,#10092);
#8893=AXIS2_PLACEMENT_3D('',#12670,#10093,#10094);
#8894=AXIS2_PLACEMENT_3D('',#12673,#10096,#10097);
#8895=AXIS2_PLACEMENT_3D('',#12674,#10098,#10099);
#8896=AXIS2_PLACEMENT_3D('',#12679,#10101,#10102);
#8897=AXIS2_PLACEMENT_3D('',#12682,#10104,#10105);
#8898=AXIS2_PLACEMENT_3D('',#12683,#10106,#10107);
#8899=AXIS2_PLACEMENT_3D('',#12699,#10115,#10116);
#8900=AXIS2_PLACEMENT_3D('',#12701,#10118,#10119);
#8901=AXIS2_PLACEMENT_3D('',#12705,#10122,#10123);
#8902=AXIS2_PLACEMENT_3D('',#12719,#10131,#10132);
#8903=AXIS2_PLACEMENT_3D('',#12725,#10136,#10137);
#8904=AXIS2_PLACEMENT_3D('',#12729,#10140,#10141);
#8905=AXIS2_PLACEMENT_3D('',#12733,#10144,#10145);
#8906=AXIS2_PLACEMENT_3D('',#12735,#10147,#10148);
#8907=AXIS2_PLACEMENT_3D('',#12739,#10151,#10152);
#8908=AXIS2_PLACEMENT_3D('',#12744,#10155,#10156);
#8909=AXIS2_PLACEMENT_3D('',#12745,#10157,#10158);
#8910=AXIS2_PLACEMENT_3D('',#12753,#10164,#10165);
#8911=AXIS2_PLACEMENT_3D('',#12754,#10166,#10167);
#8912=AXIS2_PLACEMENT_3D('',#12755,#10168,#10169);
#8913=AXIS2_PLACEMENT_3D('',#12757,#10171,#10172);
#8914=AXIS2_PLACEMENT_3D('',#12759,#10174,#10175);
#8915=AXIS2_PLACEMENT_3D('',#12760,#10176,#10177);
#8916=AXIS2_PLACEMENT_3D('',#12761,#10178,#10179);
#8917=AXIS2_PLACEMENT_3D('',#12762,#10180,#10181);
#8918=AXIS2_PLACEMENT_3D('',#12764,#10182,#10183);
#8919=AXIS2_PLACEMENT_3D('',#12767,#10185,#10186);
#8920=AXIS2_PLACEMENT_3D('',#12768,#10187,#10188);
#8921=AXIS2_PLACEMENT_3D('',#12770,#10189,#10190);
#8922=AXIS2_PLACEMENT_3D('',#12773,#10192,#10193);
#8923=AXIS2_PLACEMENT_3D('',#12774,#10194,#10195);
#8924=AXIS2_PLACEMENT_3D('',#12776,#10196,#10197);
#8925=AXIS2_PLACEMENT_3D('',#12779,#10199,#10200);
#8926=AXIS2_PLACEMENT_3D('',#12780,#10201,#10202);
#8927=AXIS2_PLACEMENT_3D('',#12782,#10203,#10204);
#8928=AXIS2_PLACEMENT_3D('',#12785,#10206,#10207);
#8929=AXIS2_PLACEMENT_3D('',#12786,#10208,#10209);
#8930=AXIS2_PLACEMENT_3D('',#12788,#10210,#10211);
#8931=AXIS2_PLACEMENT_3D('',#12791,#10213,#10214);
#8932=AXIS2_PLACEMENT_3D('',#12792,#10215,#10216);
#8933=AXIS2_PLACEMENT_3D('',#12794,#10217,#10218);
#8934=AXIS2_PLACEMENT_3D('',#12795,#10219,#10220);
#8935=AXIS2_PLACEMENT_3D('',#12798,#10222,#10223);
#8936=AXIS2_PLACEMENT_3D('',#12799,#10224,#10225);
#8937=AXIS2_PLACEMENT_3D('',#12801,#10226,#10227);
#8938=AXIS2_PLACEMENT_3D('',#12804,#10229,#10230);
#8939=AXIS2_PLACEMENT_3D('',#12805,#10231,#10232);
#8940=AXIS2_PLACEMENT_3D('',#12806,#10233,#10234);
#8941=AXIS2_PLACEMENT_3D('',#12807,#10235,#10236);
#8942=AXIS2_PLACEMENT_3D('',#12808,#10237,#10238);
#8943=AXIS2_PLACEMENT_3D('',#12810,#10239,#10240);
#8944=AXIS2_PLACEMENT_3D('',#12813,#10242,#10243);
#8945=AXIS2_PLACEMENT_3D('',#12814,#10244,#10245);
#8946=AXIS2_PLACEMENT_3D('',#12816,#10246,#10247);
#8947=AXIS2_PLACEMENT_3D('',#12819,#10249,#10250);
#8948=AXIS2_PLACEMENT_3D('',#12820,#10251,#10252);
#8949=AXIS2_PLACEMENT_3D('',#12822,#10253,#10254);
#8950=AXIS2_PLACEMENT_3D('',#12825,#10256,#10257);
#8951=AXIS2_PLACEMENT_3D('',#12826,#10258,#10259);
#8952=AXIS2_PLACEMENT_3D('',#12828,#10260,#10261);
#8953=AXIS2_PLACEMENT_3D('',#12831,#10263,#10264);
#8954=AXIS2_PLACEMENT_3D('',#12832,#10265,#10266);
#8955=AXIS2_PLACEMENT_3D('',#12834,#10267,#10268);
#8956=AXIS2_PLACEMENT_3D('',#12837,#10270,#10271);
#8957=AXIS2_PLACEMENT_3D('',#12838,#10272,#10273);
#8958=AXIS2_PLACEMENT_3D('',#12840,#10274,#10275);
#8959=AXIS2_PLACEMENT_3D('',#12841,#10276,#10277);
#8960=AXIS2_PLACEMENT_3D('',#12843,#10278,#10279);
#8961=AXIS2_PLACEMENT_3D('',#12845,#10281,#10282);
#8962=AXIS2_PLACEMENT_3D('',#12847,#10283,#10284);
#8963=AXIS2_PLACEMENT_3D('',#12850,#10286,#10287);
#8964=AXIS2_PLACEMENT_3D('',#12851,#10288,#10289);
#8965=AXIS2_PLACEMENT_3D('',#12852,#10290,#10291);
#8966=AXIS2_PLACEMENT_3D('',#12853,#10292,#10293);
#8967=AXIS2_PLACEMENT_3D('',#12854,#10294,#10295);
#8968=AXIS2_PLACEMENT_3D('',#12856,#10296,#10297);
#8969=AXIS2_PLACEMENT_3D('',#12859,#10299,#10300);
#8970=AXIS2_PLACEMENT_3D('',#12860,#10301,#10302);
#8971=AXIS2_PLACEMENT_3D('',#12862,#10303,#10304);
#8972=AXIS2_PLACEMENT_3D('',#12863,#10305,#10306);
#8973=AXIS2_PLACEMENT_3D('',#12865,#10307,#10308);
#8974=AXIS2_PLACEMENT_3D('',#12868,#10310,#10311);
#8975=AXIS2_PLACEMENT_3D('',#12869,#10312,#10313);
#8976=AXIS2_PLACEMENT_3D('',#12871,#10314,#10315);
#8977=AXIS2_PLACEMENT_3D('',#12872,#10316,#10317);
#8978=AXIS2_PLACEMENT_3D('',#12874,#10318,#10319);
#8979=AXIS2_PLACEMENT_3D('',#12877,#10321,#10322);
#8980=AXIS2_PLACEMENT_3D('',#12878,#10323,#10324);
#8981=AXIS2_PLACEMENT_3D('',#12880,#10325,#10326);
#8982=AXIS2_PLACEMENT_3D('',#12881,#10327,#10328);
#8983=AXIS2_PLACEMENT_3D('',#12883,#10329,#10330);
#8984=AXIS2_PLACEMENT_3D('',#12886,#10332,#10333);
#8985=AXIS2_PLACEMENT_3D('',#12887,#10334,#10335);
#8986=AXIS2_PLACEMENT_3D('',#12889,#10336,#10337);
#8987=AXIS2_PLACEMENT_3D('',#12890,#10338,#10339);
#8988=AXIS2_PLACEMENT_3D('',#12892,#10340,#10341);
#8989=AXIS2_PLACEMENT_3D('',#12894,#10343,#10344);
#8990=AXIS2_PLACEMENT_3D('',#12896,#10345,#10346);
#8991=AXIS2_PLACEMENT_3D('',#12898,#10348,#10349);
#8992=AXIS2_PLACEMENT_3D('',#12900,#10350,#10351);
#8993=AXIS2_PLACEMENT_3D('',#12902,#10353,#10354);
#8994=AXIS2_PLACEMENT_3D('',#12904,#10355,#10356);
#8995=AXIS2_PLACEMENT_3D('',#12906,#10358,#10359);
#8996=AXIS2_PLACEMENT_3D('',#12908,#10360,#10361);
#8997=AXIS2_PLACEMENT_3D('',#12911,#10363,#10364);
#8998=AXIS2_PLACEMENT_3D('',#12912,#10365,#10366);
#8999=AXIS2_PLACEMENT_3D('',#12914,#10367,#10368);
#9000=AXIS2_PLACEMENT_3D('',#12915,#10369,#10370);
#9001=AXIS2_PLACEMENT_3D('',#12917,#10371,#10372);
#9002=AXIS2_PLACEMENT_3D('',#12919,#10374,#10375);
#9003=AXIS2_PLACEMENT_3D('',#12921,#10376,#10377);
#9004=AXIS2_PLACEMENT_3D('',#12924,#10379,#10380);
#9005=AXIS2_PLACEMENT_3D('',#12925,#10381,#10382);
#9006=AXIS2_PLACEMENT_3D('',#12926,#10383,#10384);
#9007=AXIS2_PLACEMENT_3D('',#12927,#10385,#10386);
#9008=AXIS2_PLACEMENT_3D('',#12928,#10387,#10388);
#9009=AXIS2_PLACEMENT_3D('',#12937,#10393,#10394);
#9010=AXIS2_PLACEMENT_3D('',#12943,#10398,#10399);
#9011=AXIS2_PLACEMENT_3D('',#12949,#10403,#10404);
#9012=AXIS2_PLACEMENT_3D('',#12952,#10407,#10408);
#9013=AXIS2_PLACEMENT_3D('',#12953,#10409,#10410);
#9014=AXIS2_PLACEMENT_3D('',#12954,#10411,#10412);
#9015=AXIS2_PLACEMENT_3D('',#12955,#10413,#10414);
#9016=AXIS2_PLACEMENT_3D('',#12957,#10415,#10416);
#9017=AXIS2_PLACEMENT_3D('',#12960,#10418,#10419);
#9018=AXIS2_PLACEMENT_3D('',#12961,#10420,#10421);
#9019=AXIS2_PLACEMENT_3D('',#12962,#10422,#10423);
#9020=AXIS2_PLACEMENT_3D('',#12964,#10424,#10425);
#9021=AXIS2_PLACEMENT_3D('',#12967,#10427,#10428);
#9022=AXIS2_PLACEMENT_3D('',#12968,#10429,#10430);
#9023=AXIS2_PLACEMENT_3D('',#12969,#10431,#10432);
#9024=AXIS2_PLACEMENT_3D('',#12978,#10437,#10438);
#9025=AXIS2_PLACEMENT_3D('',#12984,#10442,#10443);
#9026=AXIS2_PLACEMENT_3D('',#12990,#10447,#10448);
#9027=AXIS2_PLACEMENT_3D('',#12993,#10451,#10452);
#9028=AXIS2_PLACEMENT_3D('',#12994,#10453,#10454);
#9029=AXIS2_PLACEMENT_3D('',#12995,#10455,#10456);
#9030=AXIS2_PLACEMENT_3D('',#12996,#10457,#10458);
#9031=AXIS2_PLACEMENT_3D('',#12998,#10459,#10460);
#9032=AXIS2_PLACEMENT_3D('',#13001,#10462,#10463);
#9033=AXIS2_PLACEMENT_3D('',#13002,#10464,#10465);
#9034=AXIS2_PLACEMENT_3D('',#13003,#10466,#10467);
#9035=AXIS2_PLACEMENT_3D('',#13005,#10468,#10469);
#9036=AXIS2_PLACEMENT_3D('',#13008,#10471,#10472);
#9037=AXIS2_PLACEMENT_3D('',#13009,#10473,#10474);
#9038=AXIS2_PLACEMENT_3D('',#13010,#10475,#10476);
#9039=AXIS2_PLACEMENT_3D('',#13019,#10481,#10482);
#9040=AXIS2_PLACEMENT_3D('',#13025,#10486,#10487);
#9041=AXIS2_PLACEMENT_3D('',#13031,#10491,#10492);
#9042=AXIS2_PLACEMENT_3D('',#13034,#10495,#10496);
#9043=AXIS2_PLACEMENT_3D('',#13035,#10497,#10498);
#9044=AXIS2_PLACEMENT_3D('',#13036,#10499,#10500);
#9045=AXIS2_PLACEMENT_3D('',#13037,#10501,#10502);
#9046=AXIS2_PLACEMENT_3D('',#13039,#10503,#10504);
#9047=AXIS2_PLACEMENT_3D('',#13042,#10506,#10507);
#9048=AXIS2_PLACEMENT_3D('',#13043,#10508,#10509);
#9049=AXIS2_PLACEMENT_3D('',#13044,#10510,#10511);
#9050=AXIS2_PLACEMENT_3D('',#13046,#10512,#10513);
#9051=AXIS2_PLACEMENT_3D('',#13048,#10514,#10515);
#9052=AXIS2_PLACEMENT_3D('',#13049,#10516,#10517);
#9053=AXIS2_PLACEMENT_3D('',#13051,#10518,#10519);
#9054=AXIS2_PLACEMENT_3D('',#13053,#10521,#10522);
#9055=AXIS2_PLACEMENT_3D('',#13054,#10523,#10524);
#9056=AXIS2_PLACEMENT_3D('',#13057,#10526,#10527);
#9057=AXIS2_PLACEMENT_3D('',#13058,#10528,#10529);
#9058=AXIS2_PLACEMENT_3D('',#13059,#10530,#10531);
#9059=AXIS2_PLACEMENT_3D('',#13060,#10532,#10533);
#9060=AXIS2_PLACEMENT_3D('',#13069,#10538,#10539);
#9061=AXIS2_PLACEMENT_3D('',#13075,#10543,#10544);
#9062=AXIS2_PLACEMENT_3D('',#13081,#10548,#10549);
#9063=AXIS2_PLACEMENT_3D('',#13087,#10553,#10554);
#9064=AXIS2_PLACEMENT_3D('',#13093,#10558,#10559);
#9065=AXIS2_PLACEMENT_3D('',#13099,#10563,#10564);
#9066=AXIS2_PLACEMENT_3D('',#13105,#10568,#10569);
#9067=AXIS2_PLACEMENT_3D('',#13111,#10573,#10574);
#9068=AXIS2_PLACEMENT_3D('',#13117,#10578,#10579);
#9069=AXIS2_PLACEMENT_3D('',#13126,#10584,#10585);
#9070=AXIS2_PLACEMENT_3D('',#13132,#10589,#10590);
#9071=AXIS2_PLACEMENT_3D('',#13138,#10594,#10595);
#9072=AXIS2_PLACEMENT_3D('',#13144,#10599,#10600);
#9073=AXIS2_PLACEMENT_3D('',#13150,#10604,#10605);
#9074=AXIS2_PLACEMENT_3D('',#13156,#10609,#10610);
#9075=AXIS2_PLACEMENT_3D('',#13162,#10614,#10615);
#9076=AXIS2_PLACEMENT_3D('',#13168,#10619,#10620);
#9077=AXIS2_PLACEMENT_3D('',#13174,#10624,#10625);
#9078=AXIS2_PLACEMENT_3D('',#13183,#10630,#10631);
#9079=AXIS2_PLACEMENT_3D('',#13189,#10635,#10636);
#9080=AXIS2_PLACEMENT_3D('',#13195,#10640,#10641);
#9081=AXIS2_PLACEMENT_3D('',#13201,#10645,#10646);
#9082=AXIS2_PLACEMENT_3D('',#13207,#10650,#10651);
#9083=AXIS2_PLACEMENT_3D('',#13213,#10655,#10656);
#9084=AXIS2_PLACEMENT_3D('',#13219,#10660,#10661);
#9085=AXIS2_PLACEMENT_3D('',#13225,#10665,#10666);
#9086=AXIS2_PLACEMENT_3D('',#13231,#10670,#10671);
#9087=AXIS2_PLACEMENT_3D('',#13240,#10676,#10677);
#9088=AXIS2_PLACEMENT_3D('',#13246,#10681,#10682);
#9089=AXIS2_PLACEMENT_3D('',#13252,#10686,#10687);
#9090=AXIS2_PLACEMENT_3D('',#13258,#10691,#10692);
#9091=AXIS2_PLACEMENT_3D('',#13264,#10696,#10697);
#9092=AXIS2_PLACEMENT_3D('',#13270,#10701,#10702);
#9093=AXIS2_PLACEMENT_3D('',#13276,#10706,#10707);
#9094=AXIS2_PLACEMENT_3D('',#13282,#10711,#10712);
#9095=AXIS2_PLACEMENT_3D('',#13288,#10716,#10717);
#9096=AXIS2_PLACEMENT_3D('',#13290,#10718,#10719);
#9097=AXIS2_PLACEMENT_3D('',#13293,#10721,#10722);
#9098=AXIS2_PLACEMENT_3D('',#13294,#10723,#10724);
#9099=AXIS2_PLACEMENT_3D('',#13300,#10728,#10729);
#9100=AXIS2_PLACEMENT_3D('',#13306,#10733,#10734);
#9101=AXIS2_PLACEMENT_3D('',#13309,#10737,#10738);
#9102=AXIS2_PLACEMENT_3D('',#13315,#10742,#10743);
#9103=AXIS2_PLACEMENT_3D('',#13318,#10746,#10747);
#9104=AXIS2_PLACEMENT_3D('',#13324,#10751,#10752);
#9105=AXIS2_PLACEMENT_3D('',#13327,#10755,#10756);
#9106=AXIS2_PLACEMENT_3D('',#13330,#10759,#10760);
#9107=AXIS2_PLACEMENT_3D('',#13331,#10761,#10762);
#9108=AXIS2_PLACEMENT_3D('',#13332,#10763,#10764);
#9109=AXIS2_PLACEMENT_3D('',#13333,#10765,#10766);
#9110=AXIS2_PLACEMENT_3D('',#13342,#10771,#10772);
#9111=AXIS2_PLACEMENT_3D('',#13348,#10776,#10777);
#9112=AXIS2_PLACEMENT_3D('',#13355,#10781,#10782);
#9113=AXIS2_PLACEMENT_3D('',#13356,#10783,#10784);
#9114=AXIS2_PLACEMENT_3D('',#13370,#10792,#10793);
#9115=AXIS2_PLACEMENT_3D('',#13374,#10796,#10797);
#9116=AXIS2_PLACEMENT_3D('',#13378,#10800,#10801);
#9117=AXIS2_PLACEMENT_3D('',#13388,#10807,#10808);
#9118=AXIS2_PLACEMENT_3D('',#13390,#10810,#10811);
#9119=AXIS2_PLACEMENT_3D('',#13394,#10813,#10814);
#9120=AXIS2_PLACEMENT_3D('',#13396,#10816,#10817);
#9121=AXIS2_PLACEMENT_3D('',#13398,#10818,#10819);
#9122=AXIS2_PLACEMENT_3D('',#13401,#10821,#10822);
#9123=AXIS2_PLACEMENT_3D('',#13403,#10823,#10824);
#9124=AXIS2_PLACEMENT_3D('',#13404,#10825,#10826);
#9125=AXIS2_PLACEMENT_3D('',#13405,#10827,#10828);
#9126=AXIS2_PLACEMENT_3D('',#13407,#10830,#10831);
#9127=AXIS2_PLACEMENT_3D('',#13409,#10833,#10834);
#9128=AXIS2_PLACEMENT_3D('',#13411,#10836,#10837);
#9129=AXIS2_PLACEMENT_3D('',#13412,#10838,#10839);
#9130=AXIS2_PLACEMENT_3D('',#13413,#10840,#10841);
#9131=AXIS2_PLACEMENT_3D('',#13415,#10842,#10843);
#9132=AXIS2_PLACEMENT_3D('',#13418,#10845,#10846);
#9133=AXIS2_PLACEMENT_3D('',#13419,#10847,#10848);
#9134=AXIS2_PLACEMENT_3D('',#13422,#10850,#10851);
#9135=AXIS2_PLACEMENT_3D('',#13423,#10852,#10853);
#9136=AXIS2_PLACEMENT_3D('',#13425,#10854,#10855);
#9137=AXIS2_PLACEMENT_3D('',#13426,#10856,#10857);
#9138=AXIS2_PLACEMENT_3D('',#13429,#10859,#10860);
#9139=AXIS2_PLACEMENT_3D('',#13430,#10861,#10862);
#9140=AXIS2_PLACEMENT_3D('',#13431,#10863,#10864);
#9141=AXIS2_PLACEMENT_3D('',#13432,#10865,#10866);
#9142=AXIS2_PLACEMENT_3D('',#13441,#10871,#10872);
#9143=AXIS2_PLACEMENT_3D('',#13447,#10876,#10877);
#9144=AXIS2_PLACEMENT_3D('',#13453,#10881,#10882);
#9145=AXIS2_PLACEMENT_3D('',#13459,#10886,#10887);
#9146=AXIS2_PLACEMENT_3D('',#13465,#10891,#10892);
#9147=AXIS2_PLACEMENT_3D('',#13468,#10895,#10896);
#9148=AXIS2_PLACEMENT_3D('',#13469,#10897,#10898);
#9149=AXIS2_PLACEMENT_3D('',#13470,#10899,#10900);
#9150=AXIS2_PLACEMENT_3D('',#13472,#10901,#10902);
#9151=AXIS2_PLACEMENT_3D('',#13473,#10903,#10904);
#9152=AXIS2_PLACEMENT_3D('',#13475,#10905,#10906);
#9153=AXIS2_PLACEMENT_3D('',#13476,#10907,#10908);
#9154=AXIS2_PLACEMENT_3D('',#13478,#10909,#10910);
#9155=AXIS2_PLACEMENT_3D('',#13480,#10912,#10913);
#9156=AXIS2_PLACEMENT_3D('',#13482,#10914,#10915);
#9157=AXIS2_PLACEMENT_3D('',#13484,#10917,#10918);
#9158=AXIS2_PLACEMENT_3D('',#13486,#10919,#10920);
#9159=AXIS2_PLACEMENT_3D('',#13488,#10922,#10923);
#9160=AXIS2_PLACEMENT_3D('',#13490,#10924,#10925);
#9161=AXIS2_PLACEMENT_3D('',#13491,#10926,#10927);
#9162=AXIS2_PLACEMENT_3D('',#13493,#10928,#10929);
#9163=AXIS2_PLACEMENT_3D('',#13495,#10931,#10932);
#9164=AXIS2_PLACEMENT_3D('',#13497,#10934,#10935);
#9165=AXIS2_PLACEMENT_3D('',#13498,#10936,#10937);
#9166=AXIS2_PLACEMENT_3D('',#13499,#10938,#10939);
#9167=AXIS2_PLACEMENT_3D('',#13502,#10940,#10941);
#9168=AXIS2_PLACEMENT_3D('',#13503,#10942,#10943);
#9169=AXIS2_PLACEMENT_3D('',#13505,#10944,#10945);
#9170=AXIS2_PLACEMENT_3D('',#13507,#10946,#10947);
#9171=AXIS2_PLACEMENT_3D('',#13508,#10948,#10949);
#9172=AXIS2_PLACEMENT_3D('',#13509,#10950,#10951);
#9173=AXIS2_PLACEMENT_3D('',#13512,#10953,#10954);
#9174=AXIS2_PLACEMENT_3D('',#13513,#10955,#10956);
#9175=AXIS2_PLACEMENT_3D('',#13515,#10957,#10958);
#9176=AXIS2_PLACEMENT_3D('',#13518,#10960,#10961);
#9177=AXIS2_PLACEMENT_3D('',#13519,#10962,#10963);
#9178=AXIS2_PLACEMENT_3D('',#13522,#10965,#10966);
#9179=AXIS2_PLACEMENT_3D('',#13523,#10967,#10968);
#9180=AXIS2_PLACEMENT_3D('',#13524,#10969,#10970);
#9181=AXIS2_PLACEMENT_3D('',#13526,#10971,#10972);
#9182=AXIS2_PLACEMENT_3D('',#13528,#10974,#10975);
#9183=AXIS2_PLACEMENT_3D('',#13530,#10976,#10977);
#9184=AXIS2_PLACEMENT_3D('',#13531,#10978,#10979);
#9185=AXIS2_PLACEMENT_3D('',#13533,#10981,#10982);
#9186=AXIS2_PLACEMENT_3D('',#13534,#10983,#10984);
#9187=AXIS2_PLACEMENT_3D('',#13537,#10985,#10986);
#9188=AXIS2_PLACEMENT_3D('',#13538,#10987,#10988);
#9189=AXIS2_PLACEMENT_3D('',#13540,#10989,#10990);
#9190=AXIS2_PLACEMENT_3D('',#13542,#10991,#10992);
#9191=AXIS2_PLACEMENT_3D('',#13543,#10993,#10994);
#9192=AXIS2_PLACEMENT_3D('',#13544,#10995,#10996);
#9193=AXIS2_PLACEMENT_3D('',#13546,#10997,#10998);
#9194=AXIS2_PLACEMENT_3D('',#13548,#11000,#11001);
#9195=AXIS2_PLACEMENT_3D('',#13550,#11002,#11003);
#9196=AXIS2_PLACEMENT_3D('',#13552,#11004,#11005);
#9197=AXIS2_PLACEMENT_3D('',#13553,#11006,#11007);
#9198=AXIS2_PLACEMENT_3D('',#13555,#11008,#11009);
#9199=AXIS2_PLACEMENT_3D('',#13557,#11011,#11012);
#9200=AXIS2_PLACEMENT_3D('',#13559,#11013,#11014);
#9201=AXIS2_PLACEMENT_3D('',#13561,#11016,#11017);
#9202=AXIS2_PLACEMENT_3D('',#13563,#11018,#11019);
#9203=AXIS2_PLACEMENT_3D('',#13565,#11021,#11022);
#9204=AXIS2_PLACEMENT_3D('',#13566,#11023,#11024);
#9205=AXIS2_PLACEMENT_3D('',#13568,#11026,#11027);
#9206=AXIS2_PLACEMENT_3D('',#13569,#11028,#11029);
#9207=AXIS2_PLACEMENT_3D('',#13572,#11030,#11031);
#9208=AXIS2_PLACEMENT_3D('',#13573,#11032,#11033);
#9209=AXIS2_PLACEMENT_3D('',#13576,#11034,#11035);
#9210=AXIS2_PLACEMENT_3D('',#13577,#11036,#11037);
#9211=AXIS2_PLACEMENT_3D('',#13580,#11038,#11039);
#9212=AXIS2_PLACEMENT_3D('',#13581,#11040,#11041);
#9213=AXIS2_PLACEMENT_3D('',#13584,#11042,#11043);
#9214=AXIS2_PLACEMENT_3D('',#13585,#11044,#11045);
#9215=AXIS2_PLACEMENT_3D('',#13588,#11046,#11047);
#9216=AXIS2_PLACEMENT_3D('',#13589,#11048,#11049);
#9217=AXIS2_PLACEMENT_3D('',#13592,#11050,#11051);
#9218=AXIS2_PLACEMENT_3D('',#13593,#11052,#11053);
#9219=AXIS2_PLACEMENT_3D('',#13596,#11054,#11055);
#9220=AXIS2_PLACEMENT_3D('',#13597,#11056,#11057);
#9221=AXIS2_PLACEMENT_3D('',#13600,#11058,#11059);
#9222=AXIS2_PLACEMENT_3D('',#13601,#11060,#11061);
#9223=AXIS2_PLACEMENT_3D('',#13602,#11062,#11063);
#9224=AXIS2_PLACEMENT_3D('',#13628,#11064,#11065);
#9225=AXIS2_PLACEMENT_3D('',#13652,#11066,#11067);
#9226=AXIS2_PLACEMENT_3D('',#13653,#11068,#11069);
#9227=AXIS2_PLACEMENT_3D('',#13655,#11070,#11071);
#9228=AXIS2_PLACEMENT_3D('',#13680,#11072,#11073);
#9229=AXIS2_PLACEMENT_3D('',#13705,#11074,#11075);
#9230=AXIS2_PLACEMENT_3D('',#13721,#11077,#11078);
#9231=AXIS2_PLACEMENT_3D('',#13736,#11079,#11080);
#9232=AXIS2_PLACEMENT_3D('',#13761,#11081,#11082);
#9233=AXIS2_PLACEMENT_3D('',#13786,#11083,#11084);
#9234=AXIS2_PLACEMENT_3D('',#13811,#11085,#11086);
#9235=AXIS2_PLACEMENT_3D('',#13835,#11087,#11088);
#9236=AXIS2_PLACEMENT_3D('',#13836,#11089,#11090);
#9237=AXIS2_PLACEMENT_3D('',#13838,#11091,#11092);
#9238=AXIS2_PLACEMENT_3D('',#13839,#11093,#11094);
#9239=AXIS2_PLACEMENT_3D('',#13840,#11095,#11096);
#9240=AXIS2_PLACEMENT_3D('',#13864,#11097,#11098);
#9241=AXIS2_PLACEMENT_3D('',#13865,#11099,#11100);
#9242=AXIS2_PLACEMENT_3D('',#13867,#11101,#11102);
#9243=AXIS2_PLACEMENT_3D('',#13868,#11103,#11104);
#9244=AXIS2_PLACEMENT_3D('',#13869,#11105,#11106);
#9245=AXIS2_PLACEMENT_3D('',#13893,#11107,#11108);
#9246=AXIS2_PLACEMENT_3D('',#13894,#11109,#11110);
#9247=AXIS2_PLACEMENT_3D('',#13896,#11111,#11112);
#9248=AXIS2_PLACEMENT_3D('',#13897,#11113,#11114);
#9249=AXIS2_PLACEMENT_3D('',#13898,#11115,#11116);
#9250=AXIS2_PLACEMENT_3D('',#13913,#11117,#11118);
#9251=AXIS2_PLACEMENT_3D('',#13926,#11119,#11120);
#9252=AXIS2_PLACEMENT_3D('',#13928,#11121,#11122);
#9253=AXIS2_PLACEMENT_3D('',#13929,#11123,#11124);
#9254=AXIS2_PLACEMENT_3D('',#13930,#11125,#11126);
#9255=AXIS2_PLACEMENT_3D('',#13954,#11127,#11128);
#9256=AXIS2_PLACEMENT_3D('',#13955,#11129,#11130);
#9257=AXIS2_PLACEMENT_3D('',#13957,#11131,#11132);
#9258=AXIS2_PLACEMENT_3D('',#13958,#11133,#11134);
#9259=AXIS2_PLACEMENT_3D('',#13959,#11135,#11136);
#9260=AXIS2_PLACEMENT_3D('',#13983,#11137,#11138);
#9261=AXIS2_PLACEMENT_3D('',#13984,#11139,#11140);
#9262=AXIS2_PLACEMENT_3D('',#13986,#11141,#11142);
#9263=AXIS2_PLACEMENT_3D('',#13987,#11143,#11144);
#9264=AXIS2_PLACEMENT_3D('',#13988,#11145,#11146);
#9265=AXIS2_PLACEMENT_3D('',#14012,#11147,#11148);
#9266=AXIS2_PLACEMENT_3D('',#14013,#11149,#11150);
#9267=AXIS2_PLACEMENT_3D('',#14015,#11151,#11152);
#9268=AXIS2_PLACEMENT_3D('',#14018,#11154,#11155);
#9269=AXIS2_PLACEMENT_3D('',#14042,#11156,#11157);
#9270=AXIS2_PLACEMENT_3D('',#14043,#11158,#11159);
#9271=AXIS2_PLACEMENT_3D('',#14044,#11160,#11161);
#9272=AXIS2_PLACEMENT_3D('',#14045,#11162,#11163);
#9273=AXIS2_PLACEMENT_3D('',#14046,#11164,#11165);
#9274=AXIS2_PLACEMENT_3D('',#14047,#11166,#11167);
#9275=AXIS2_PLACEMENT_3D('',#14048,#11168,#11169);
#9276=AXIS2_PLACEMENT_3D('',#14049,#11170,#11171);
#9277=AXIS2_PLACEMENT_3D('',#14050,#11172,#11173);
#9278=AXIS2_PLACEMENT_3D('',#14052,#11174,#11175);
#9279=AXIS2_PLACEMENT_3D('',#14054,#11176,#11177);
#9280=AXIS2_PLACEMENT_3D('',#14055,#11178,#11179);
#9281=AXIS2_PLACEMENT_3D('',#14057,#11180,#11181);
#9282=AXIS2_PLACEMENT_3D('',#14059,#11183,#11184);
#9283=AXIS2_PLACEMENT_3D('',#14061,#11185,#11186);
#9284=AXIS2_PLACEMENT_3D('',#14062,#11187,#11188);
#9285=AXIS2_PLACEMENT_3D('',#14064,#11190,#11191);
#9286=AXIS2_PLACEMENT_3D('',#14066,#11192,#11193);
#9287=AXIS2_PLACEMENT_3D('',#14068,#11194,#11195);
#9288=AXIS2_PLACEMENT_3D('',#14069,#11196,#11197);
#9289=AXIS2_PLACEMENT_3D('',#14071,#11198,#11199);
#9290=AXIS2_PLACEMENT_3D('',#14073,#11201,#11202);
#9291=AXIS2_PLACEMENT_3D('',#14075,#11203,#11204);
#9292=AXIS2_PLACEMENT_3D('',#14076,#11205,#11206);
#9293=AXIS2_PLACEMENT_3D('',#14078,#11208,#11209);
#9294=AXIS2_PLACEMENT_3D('',#14079,#11210,#11211);
#9295=AXIS2_PLACEMENT_3D('',#14080,#11212,#11213);
#9296=AXIS2_PLACEMENT_3D('',#14081,#11214,#11215);
#9297=AXIS2_PLACEMENT_3D('',#14082,#11216,#11217);
#9298=AXIS2_PLACEMENT_3D('',#14083,#11218,#11219);
#9299=AXIS2_PLACEMENT_3D('',#14084,#11220,#11221);
#9300=AXIS2_PLACEMENT_3D('',#14085,#11222,#11223);
#9301=AXIS2_PLACEMENT_3D('',#14088,#11224,#11225);
#9302=AXIS2_PLACEMENT_3D('',#14094,#11229,#11230);
#9303=AXIS2_PLACEMENT_3D('',#14100,#11234,#11235);
#9304=AXIS2_PLACEMENT_3D('',#14102,#11236,#11237);
#9305=AXIS2_PLACEMENT_3D('',#14106,#11240,#11241);
#9306=AXIS2_PLACEMENT_3D('',#14109,#11244,#11245);
#9307=AXIS2_PLACEMENT_3D('',#14110,#11246,#11247);
#9308=AXIS2_PLACEMENT_3D('',#14112,#11248,#11249);
#9309=AXIS2_PLACEMENT_3D('',#14114,#11250,#11251);
#9310=AXIS2_PLACEMENT_3D('',#14115,#11252,#11253);
#9311=AXIS2_PLACEMENT_3D('',#14117,#11254,#11255);
#9312=AXIS2_PLACEMENT_3D('',#14119,#11257,#11258);
#9313=AXIS2_PLACEMENT_3D('',#14121,#11259,#11260);
#9314=AXIS2_PLACEMENT_3D('',#14122,#11261,#11262);
#9315=AXIS2_PLACEMENT_3D('',#14124,#11263,#11264);
#9316=AXIS2_PLACEMENT_3D('',#14126,#11266,#11267);
#9317=AXIS2_PLACEMENT_3D('',#14128,#11268,#11269);
#9318=AXIS2_PLACEMENT_3D('',#14129,#11270,#11271);
#9319=AXIS2_PLACEMENT_3D('',#14131,#11272,#11273);
#9320=AXIS2_PLACEMENT_3D('',#14133,#11275,#11276);
#9321=AXIS2_PLACEMENT_3D('',#14135,#11277,#11278);
#9322=AXIS2_PLACEMENT_3D('',#14136,#11279,#11280);
#9323=AXIS2_PLACEMENT_3D('',#14138,#11281,#11282);
#9324=AXIS2_PLACEMENT_3D('',#14140,#11284,#11285);
#9325=AXIS2_PLACEMENT_3D('',#14142,#11286,#11287);
#9326=AXIS2_PLACEMENT_3D('',#14143,#11288,#11289);
#9327=AXIS2_PLACEMENT_3D('',#14145,#11290,#11291);
#9328=AXIS2_PLACEMENT_3D('',#14147,#11293,#11294);
#9329=AXIS2_PLACEMENT_3D('',#14149,#11295,#11296);
#9330=AXIS2_PLACEMENT_3D('',#14150,#11297,#11298);
#9331=AXIS2_PLACEMENT_3D('',#14152,#11300,#11301);
#9332=AXIS2_PLACEMENT_3D('',#14153,#11302,#11303);
#9333=AXIS2_PLACEMENT_3D('',#14156,#11304,#11305);
#9334=AXIS2_PLACEMENT_3D('',#14160,#11307,#11308);
#9335=AXIS2_PLACEMENT_3D('',#14162,#11310,#11311);
#9336=AXIS2_PLACEMENT_3D('',#14168,#11315,#11316);
#9337=AXIS2_PLACEMENT_3D('',#14170,#11317,#11318);
#9338=AXIS2_PLACEMENT_3D('',#14172,#11319,#11320);
#9339=AXIS2_PLACEMENT_3D('',#14174,#11322,#11323);
#9340=AXIS2_PLACEMENT_3D('',#14177,#11326,#11327);
#9341=AXIS2_PLACEMENT_3D('',#14179,#11328,#11329);
#9342=AXIS2_PLACEMENT_3D('',#14181,#11330,#11331);
#9343=AXIS2_PLACEMENT_3D('',#14182,#11332,#11333);
#9344=AXIS2_PLACEMENT_3D('',#14184,#11334,#11335);
#9345=AXIS2_PLACEMENT_3D('',#14186,#11337,#11338);
#9346=AXIS2_PLACEMENT_3D('',#14188,#11339,#11340);
#9347=AXIS2_PLACEMENT_3D('',#14189,#11341,#11342);
#9348=AXIS2_PLACEMENT_3D('',#14191,#11344,#11345);
#9349=AXIS2_PLACEMENT_3D('',#14192,#11346,#11347);
#9350=AXIS2_PLACEMENT_3D('',#14193,#11348,#11349);
#9351=AXIS2_PLACEMENT_3D('',#14194,#11350,#11351);
#9352=AXIS2_PLACEMENT_3D('',#14203,#11356,#11357);
#9353=AXIS2_PLACEMENT_3D('',#14209,#11361,#11362);
#9354=AXIS2_PLACEMENT_3D('',#14215,#11366,#11367);
#9355=AXIS2_PLACEMENT_3D('',#14221,#11371,#11372);
#9356=AXIS2_PLACEMENT_3D('',#14227,#11376,#11377);
#9357=AXIS2_PLACEMENT_3D('',#14230,#11380,#11381);
#9358=AXIS2_PLACEMENT_3D('',#14231,#11382,#11383);
#9359=AXIS2_PLACEMENT_3D('',#14232,#11384,#11385);
#9360=AXIS2_PLACEMENT_3D('',#14234,#11386,#11387);
#9361=AXIS2_PLACEMENT_3D('',#14236,#11388,#11389);
#9362=AXIS2_PLACEMENT_3D('',#14237,#11390,#11391);
#9363=AXIS2_PLACEMENT_3D('',#14240,#11393,#11394);
#9364=AXIS2_PLACEMENT_3D('',#14241,#11395,#11396);
#9365=AXIS2_PLACEMENT_3D('',#14242,#11397,#11398);
#9366=AXIS2_PLACEMENT_3D('',#14244,#11399,#11400);
#9367=AXIS2_PLACEMENT_3D('',#14245,#11401,#11402);
#9368=AXIS2_PLACEMENT_3D('',#14247,#11403,#11404);
#9369=AXIS2_PLACEMENT_3D('',#14249,#11406,#11407);
#9370=AXIS2_PLACEMENT_3D('',#14251,#11408,#11409);
#9371=AXIS2_PLACEMENT_3D('',#14253,#11411,#11412);
#9372=AXIS2_PLACEMENT_3D('',#14255,#11413,#11414);
#9373=AXIS2_PLACEMENT_3D('',#14257,#11416,#11417);
#9374=AXIS2_PLACEMENT_3D('',#14259,#11418,#11419);
#9375=AXIS2_PLACEMENT_3D('',#14260,#11420,#11421);
#9376=AXIS2_PLACEMENT_3D('',#14262,#11422,#11423);
#9377=AXIS2_PLACEMENT_3D('',#14264,#11425,#11426);
#9378=AXIS2_PLACEMENT_3D('',#14266,#11427,#11428);
#9379=AXIS2_PLACEMENT_3D('',#14268,#11430,#11431);
#9380=AXIS2_PLACEMENT_3D('',#14270,#11433,#11434);
#9381=AXIS2_PLACEMENT_3D('',#14271,#11435,#11436);
#9382=AXIS2_PLACEMENT_3D('',#14272,#11437,#11438);
#9383=AXIS2_PLACEMENT_3D('',#14274,#11439,#11440);
#9384=AXIS2_PLACEMENT_3D('',#14277,#11442,#11443);
#9385=AXIS2_PLACEMENT_3D('',#14278,#11444,#11445);
#9386=AXIS2_PLACEMENT_3D('',#14283,#11447,#11448);
#9387=AXIS2_PLACEMENT_3D('',#14286,#11450,#11451);
#9388=AXIS2_PLACEMENT_3D('',#14287,#11452,#11453);
#9389=AXIS2_PLACEMENT_3D('',#14291,#11455,#11456);
#9390=AXIS2_PLACEMENT_3D('',#14293,#11457,#11458);
#9391=AXIS2_PLACEMENT_3D('',#14297,#11460,#11461);
#9392=AXIS2_PLACEMENT_3D('',#14301,#11463,#11464);
#9393=AXIS2_PLACEMENT_3D('',#14304,#11466,#11467);
#9394=AXIS2_PLACEMENT_3D('',#14305,#11468,#11469);
#9395=AXIS2_PLACEMENT_3D('',#14309,#11472,#11473);
#9396=AXIS2_PLACEMENT_3D('',#14312,#11475,#11476);
#9397=AXIS2_PLACEMENT_3D('',#14313,#11477,#11478);
#9398=AXIS2_PLACEMENT_3D('',#14315,#11480,#11481);
#9399=AXIS2_PLACEMENT_3D('',#14319,#11483,#11484);
#9400=AXIS2_PLACEMENT_3D('',#14321,#11486,#11487);
#9401=AXIS2_PLACEMENT_3D('',#14325,#11490,#11491);
#9402=AXIS2_PLACEMENT_3D('',#14328,#11493,#11494);
#9403=AXIS2_PLACEMENT_3D('',#14329,#11495,#11496);
#9404=AXIS2_PLACEMENT_3D('',#14331,#11498,#11499);
#9405=AXIS2_PLACEMENT_3D('',#14333,#11500,#11501);
#9406=AXIS2_PLACEMENT_3D('',#14335,#11502,#11503);
#9407=AXIS2_PLACEMENT_3D('',#14336,#11504,#11505);
#9408=AXIS2_PLACEMENT_3D('',#14338,#11507,#11508);
#9409=AXIS2_PLACEMENT_3D('',#14340,#11509,#11510);
#9410=AXIS2_PLACEMENT_3D('',#14342,#11511,#11512);
#9411=AXIS2_PLACEMENT_3D('',#14343,#11513,#11514);
#9412=AXIS2_PLACEMENT_3D('',#14345,#11516,#11517);
#9413=AXIS2_PLACEMENT_3D('',#14348,#11519,#11520);
#9414=AXIS2_PLACEMENT_3D('',#14349,#11521,#11522);
#9415=AXIS2_PLACEMENT_3D('',#14351,#11523,#11524);
#9416=AXIS2_PLACEMENT_3D('',#14353,#11526,#11527);
#9417=AXIS2_PLACEMENT_3D('',#14354,#11528,#11529);
#9418=AXIS2_PLACEMENT_3D('',#14355,#11530,#11531);
#9419=AXIS2_PLACEMENT_3D('',#14356,#11532,#11533);
#9420=AXIS2_PLACEMENT_3D('',#14358,#11534,#11535);
#9421=AXIS2_PLACEMENT_3D('',#14361,#11537,#11538);
#9422=AXIS2_PLACEMENT_3D('',#14362,#11539,#11540);
#9423=AXIS2_PLACEMENT_3D('',#14364,#11541,#11542);
#9424=AXIS2_PLACEMENT_3D('',#14367,#11544,#11545);
#9425=AXIS2_PLACEMENT_3D('',#14368,#11546,#11547);
#9426=AXIS2_PLACEMENT_3D('',#14369,#11548,#11549);
#9427=AXIS2_PLACEMENT_3D('',#14370,#11550,#11551);
#9428=AXIS2_PLACEMENT_3D('',#14371,#11552,#11553);
#9429=AXIS2_PLACEMENT_3D('',#14375,#11555,#11556);
#9430=AXIS2_PLACEMENT_3D('',#14376,#11557,#11558);
#9431=AXIS2_PLACEMENT_3D('',#14393,#11559,#11560);
#9432=AXIS2_PLACEMENT_3D('',#14434,#11562,#11563);
#9433=AXIS2_PLACEMENT_3D('',#14449,#11564,#11565);
#9434=AXIS2_PLACEMENT_3D('',#14451,#11567,#11568);
#9435=AXIS2_PLACEMENT_3D('',#14453,#11569,#11570);
#9436=AXIS2_PLACEMENT_3D('',#14456,#11572,#11573);
#9437=AXIS2_PLACEMENT_3D('',#14457,#11574,#11575);
#9438=AXIS2_PLACEMENT_3D('',#14459,#11576,#11577);
#9439=AXIS2_PLACEMENT_3D('',#14462,#11579,#11580);
#9440=AXIS2_PLACEMENT_3D('',#14463,#11581,#11582);
#9441=AXIS2_PLACEMENT_3D('',#14464,#11583,#11584);
#9442=AXIS2_PLACEMENT_3D('',#14465,#11585,#11586);
#9443=AXIS2_PLACEMENT_3D('',#14466,#11587,#11588);
#9444=AXIS2_PLACEMENT_3D('',#14468,#11589,#11590);
#9445=AXIS2_PLACEMENT_3D('',#14471,#11592,#11593);
#9446=AXIS2_PLACEMENT_3D('',#14472,#11594,#11595);
#9447=AXIS2_PLACEMENT_3D('',#14473,#11596,#11597);
#9448=AXIS2_PLACEMENT_3D('',#14475,#11598,#11599);
#9449=AXIS2_PLACEMENT_3D('',#14478,#11601,#11602);
#9450=AXIS2_PLACEMENT_3D('',#14479,#11603,#11604);
#9451=AXIS2_PLACEMENT_3D('',#14480,#11605,#11606);
#9452=AXIS2_PLACEMENT_3D('',#14482,#11607,#11608);
#9453=AXIS2_PLACEMENT_3D('',#14484,#11609,#11610);
#9454=AXIS2_PLACEMENT_3D('',#14485,#11611,#11612);
#9455=AXIS2_PLACEMENT_3D('',#14487,#11613,#11614);
#9456=AXIS2_PLACEMENT_3D('',#14489,#11615,#11616);
#9457=AXIS2_PLACEMENT_3D('',#14490,#11617,#11618);
#9458=AXIS2_PLACEMENT_3D('',#14492,#11620,#11621);
#9459=AXIS2_PLACEMENT_3D('',#14495,#11623,#11624);
#9460=AXIS2_PLACEMENT_3D('',#14496,#11625,#11626);
#9461=AXIS2_PLACEMENT_3D('',#14498,#11627,#11628);
#9462=AXIS2_PLACEMENT_3D('',#14500,#11630,#11631);
#9463=AXIS2_PLACEMENT_3D('',#14501,#11632,#11633);
#9464=AXIS2_PLACEMENT_3D('',#14502,#11634,#11635);
#9465=AXIS2_PLACEMENT_3D('',#14503,#11636,#11637);
#9466=AXIS2_PLACEMENT_3D('',#14505,#11638,#11639);
#9467=AXIS2_PLACEMENT_3D('',#14508,#11641,#11642);
#9468=AXIS2_PLACEMENT_3D('',#14509,#11643,#11644);
#9469=AXIS2_PLACEMENT_3D('',#14511,#11645,#11646);
#9470=AXIS2_PLACEMENT_3D('',#14514,#11648,#11649);
#9471=AXIS2_PLACEMENT_3D('',#14515,#11650,#11651);
#9472=AXIS2_PLACEMENT_3D('',#14516,#11652,#11653);
#9473=AXIS2_PLACEMENT_3D('',#14517,#11654,#11655);
#9474=AXIS2_PLACEMENT_3D('',#14518,#11656,#11657);
#9475=AXIS2_PLACEMENT_3D('',#14520,#11658,#11659);
#9476=AXIS2_PLACEMENT_3D('',#14523,#11661,#11662);
#9477=AXIS2_PLACEMENT_3D('',#14524,#11663,#11664);
#9478=AXIS2_PLACEMENT_3D('',#14526,#11665,#11666);
#9479=AXIS2_PLACEMENT_3D('',#14529,#11668,#11669);
#9480=AXIS2_PLACEMENT_3D('',#14530,#11670,#11671);
#9481=AXIS2_PLACEMENT_3D('',#14531,#11672,#11673);
#9482=AXIS2_PLACEMENT_3D('',#14532,#11674,#11675);
#9483=AXIS2_PLACEMENT_3D('',#14533,#11676,#11677);
#9484=AXIS2_PLACEMENT_3D('',#14535,#11678,#11679);
#9485=AXIS2_PLACEMENT_3D('',#14538,#11681,#11682);
#9486=AXIS2_PLACEMENT_3D('',#14539,#11683,#11684);
#9487=AXIS2_PLACEMENT_3D('',#14541,#11685,#11686);
#9488=AXIS2_PLACEMENT_3D('',#14544,#11688,#11689);
#9489=AXIS2_PLACEMENT_3D('',#14545,#11690,#11691);
#9490=AXIS2_PLACEMENT_3D('',#14546,#11692,#11693);
#9491=AXIS2_PLACEMENT_3D('',#14547,#11694,#11695);
#9492=AXIS2_PLACEMENT_3D('',#14548,#11696,#11697);
#9493=AXIS2_PLACEMENT_3D('',#14550,#11698,#11699);
#9494=AXIS2_PLACEMENT_3D('',#14553,#11701,#11702);
#9495=AXIS2_PLACEMENT_3D('',#14554,#11703,#11704);
#9496=AXIS2_PLACEMENT_3D('',#14556,#11705,#11706);
#9497=AXIS2_PLACEMENT_3D('',#14559,#11708,#11709);
#9498=AXIS2_PLACEMENT_3D('',#14560,#11710,#11711);
#9499=AXIS2_PLACEMENT_3D('',#14561,#11712,#11713);
#9500=AXIS2_PLACEMENT_3D('',#14562,#11714,#11715);
#9501=AXIS2_PLACEMENT_3D('',#14563,#11716,#11717);
#9502=AXIS2_PLACEMENT_3D('',#14565,#11718,#11719);
#9503=AXIS2_PLACEMENT_3D('',#14566,#11720,#11721);
#9504=AXIS2_PLACEMENT_3D('',#14575,#11726,#11727);
#9505=AXIS2_PLACEMENT_3D('',#14581,#11731,#11732);
#9506=AXIS2_PLACEMENT_3D('',#14587,#11736,#11737);
#9507=AXIS2_PLACEMENT_3D('',#14593,#11741,#11742);
#9508=AXIS2_PLACEMENT_3D('',#14599,#11746,#11747);
#9509=AXIS2_PLACEMENT_3D('',#14602,#11750,#11751);
#9510=AXIS2_PLACEMENT_3D('',#14603,#11752,#11753);
#9511=AXIS2_PLACEMENT_3D('',#14605,#11754,#11755);
#9512=AXIS2_PLACEMENT_3D('',#14606,#11756,#11757);
#9513=AXIS2_PLACEMENT_3D('',#14608,#11758,#11759);
#9514=AXIS2_PLACEMENT_3D('',#14610,#11761,#11762);
#9515=AXIS2_PLACEMENT_3D('',#14612,#11764,#11765);
#9516=AXIS2_PLACEMENT_3D('',#14613,#11766,#11767);
#9517=AXIS2_PLACEMENT_3D('',#14622,#11772,#11773);
#9518=AXIS2_PLACEMENT_3D('',#14628,#11777,#11778);
#9519=AXIS2_PLACEMENT_3D('',#14634,#11782,#11783);
#9520=AXIS2_PLACEMENT_3D('',#14640,#11787,#11788);
#9521=AXIS2_PLACEMENT_3D('',#14646,#11792,#11793);
#9522=AXIS2_PLACEMENT_3D('',#14649,#11796,#11797);
#9523=AXIS2_PLACEMENT_3D('',#14650,#11798,#11799);
#9524=AXIS2_PLACEMENT_3D('',#14651,#11800,#11801);
#9525=AXIS2_PLACEMENT_3D('',#14653,#11802,#11803);
#9526=AXIS2_PLACEMENT_3D('',#14654,#11804,#11805);
#9527=AXIS2_PLACEMENT_3D('',#14656,#11806,#11807);
#9528=AXIS2_PLACEMENT_3D('',#14657,#11808,#11809);
#9529=AXIS2_PLACEMENT_3D('',#14659,#11810,#11811);
#9530=AXIS2_PLACEMENT_3D('',#14661,#11813,#11814);
#9531=AXIS2_PLACEMENT_3D('',#14663,#11815,#11816);
#9532=AXIS2_PLACEMENT_3D('',#14665,#11818,#11819);
#9533=AXIS2_PLACEMENT_3D('',#14667,#11820,#11821);
#9534=AXIS2_PLACEMENT_3D('',#14669,#11823,#11824);
#9535=AXIS2_PLACEMENT_3D('',#14671,#11825,#11826);
#9536=AXIS2_PLACEMENT_3D('',#14672,#11827,#11828);
#9537=AXIS2_PLACEMENT_3D('',#14674,#11829,#11830);
#9538=AXIS2_PLACEMENT_3D('',#14676,#11832,#11833);
#9539=AXIS2_PLACEMENT_3D('',#14678,#11835,#11836);
#9540=AXIS2_PLACEMENT_3D('',#14679,#11837,#11838);
#9541=AXIS2_PLACEMENT_3D('',#14681,#11839,#11840);
#9542=AXIS2_PLACEMENT_3D('',#14682,#11841,#11842);
#9543=AXIS2_PLACEMENT_3D('',#14684,#11843,#11844);
#9544=AXIS2_PLACEMENT_3D('',#14686,#11846,#11847);
#9545=AXIS2_PLACEMENT_3D('',#14688,#11848,#11849);
#9546=AXIS2_PLACEMENT_3D('',#14690,#11851,#11852);
#9547=AXIS2_PLACEMENT_3D('',#14692,#11853,#11854);
#9548=AXIS2_PLACEMENT_3D('',#14694,#11856,#11857);
#9549=AXIS2_PLACEMENT_3D('',#14696,#11858,#11859);
#9550=AXIS2_PLACEMENT_3D('',#14697,#11860,#11861);
#9551=AXIS2_PLACEMENT_3D('',#14699,#11862,#11863);
#9552=AXIS2_PLACEMENT_3D('',#14701,#11865,#11866);
#9553=AXIS2_PLACEMENT_3D('',#14703,#11867,#11868);
#9554=AXIS2_PLACEMENT_3D('',#14705,#11870,#11871);
#9555=AXIS2_PLACEMENT_3D('',#14707,#11872,#11873);
#9556=AXIS2_PLACEMENT_3D('',#14709,#11875,#11876);
#9557=AXIS2_PLACEMENT_3D('',#14710,#11877,#11878);
#9558=AXIS2_PLACEMENT_3D('',#14719,#11883,#11884);
#9559=AXIS2_PLACEMENT_3D('',#14725,#11888,#11889);
#9560=AXIS2_PLACEMENT_3D('',#14731,#11893,#11894);
#9561=AXIS2_PLACEMENT_3D('',#14737,#11898,#11899);
#9562=AXIS2_PLACEMENT_3D('',#14743,#11903,#11904);
#9563=AXIS2_PLACEMENT_3D('',#14746,#11907,#11908);
#9564=AXIS2_PLACEMENT_3D('',#14747,#11909,#11910);
#9565=AXIS2_PLACEMENT_3D('',#14748,#11911,#11912);
#9566=AXIS2_PLACEMENT_3D('',#14749,#11913,#11914);
#9567=AXIS2_PLACEMENT_3D('',#14750,#11915,#11916);
#9568=AXIS2_PLACEMENT_3D('',#14751,#11917,#11918);
#9569=AXIS2_PLACEMENT_3D('',#14752,#11919,#11920);
#9570=AXIS2_PLACEMENT_3D('',#14753,#11921,#11922);
#9571=AXIS2_PLACEMENT_3D('',#14754,#11923,#11924);
#9572=AXIS2_PLACEMENT_3D('',#14755,#11925,#11926);
#9573=AXIS2_PLACEMENT_3D('',#14756,#11927,#11928);
#9574=AXIS2_PLACEMENT_3D('',#14757,#11929,#11930);
#9575=AXIS2_PLACEMENT_3D('',#14758,#11931,#11932);
#9576=AXIS2_PLACEMENT_3D('',#14759,#11933,#11934);
#9577=AXIS2_PLACEMENT_3D('',#14760,#11935,#11936);
#9578=AXIS2_PLACEMENT_3D('',#14761,#11937,#11938);
#9579=AXIS2_PLACEMENT_3D('',#14762,#11939,#11940);
#9580=AXIS2_PLACEMENT_3D('',#14763,#11941,#11942);
#9581=AXIS2_PLACEMENT_3D('',#14764,#11943,#11944);
#9582=AXIS2_PLACEMENT_3D('',#14765,#11945,#11946);
#9583=AXIS2_PLACEMENT_3D('',#14766,#11947,#11948);
#9584=AXIS2_PLACEMENT_3D('',#14767,#11949,#11950);
#9585=AXIS2_PLACEMENT_3D('',#14768,#11951,#11952);
#9586=AXIS2_PLACEMENT_3D('',#14769,#11953,#11954);
#9587=AXIS2_PLACEMENT_3D('',#14770,#11955,#11956);
#9588=AXIS2_PLACEMENT_3D('',#14771,#11957,#11958);
#9589=AXIS2_PLACEMENT_3D('',#14772,#11959,#11960);
#9590=AXIS2_PLACEMENT_3D('',#14773,#11961,#11962);
#9591=AXIS2_PLACEMENT_3D('',#14774,#11963,#11964);
#9592=AXIS2_PLACEMENT_3D('',#14775,#11965,#11966);
#9593=AXIS2_PLACEMENT_3D('',#14776,#11967,#11968);
#9594=AXIS2_PLACEMENT_3D('',#14777,#11969,#11970);
#9595=AXIS2_PLACEMENT_3D('',#14778,#11971,#11972);
#9596=AXIS2_PLACEMENT_3D('',#14779,#11973,#11974);
#9597=AXIS2_PLACEMENT_3D('',#14780,#11975,#11976);
#9598=AXIS2_PLACEMENT_3D('',#14781,#11977,#11978);
#9599=AXIS2_PLACEMENT_3D('',#14782,#11979,#11980);
#9600=AXIS2_PLACEMENT_3D('',#14783,#11981,#11982);
#9601=AXIS2_PLACEMENT_3D('',#14784,#11983,#11984);
#9602=AXIS2_PLACEMENT_3D('',#14785,#11985,#11986);
#9603=AXIS2_PLACEMENT_3D('',#14786,#11987,#11988);
#9604=AXIS2_PLACEMENT_3D('',#14787,#11989,#11990);
#9605=AXIS2_PLACEMENT_3D('',#14788,#11991,#11992);
#9606=AXIS2_PLACEMENT_3D('',#14789,#11993,#11994);
#9607=AXIS2_PLACEMENT_3D('',#14790,#11995,#11996);
#9608=AXIS2_PLACEMENT_3D('',#14791,#11997,#11998);
#9609=AXIS2_PLACEMENT_3D('',#14792,#11999,#12000);
#9610=AXIS2_PLACEMENT_3D('',#14793,#12001,#12002);
#9611=AXIS2_PLACEMENT_3D('',#14794,#12003,#12004);
#9612=AXIS2_PLACEMENT_3D('',#14795,#12005,#12006);
#9613=AXIS2_PLACEMENT_3D('',#14796,#12007,#12008);
#9614=AXIS2_PLACEMENT_3D('',#14797,#12009,#12010);
#9615=AXIS2_PLACEMENT_3D('',#14798,#12011,#12012);
#9616=AXIS2_PLACEMENT_3D('',#14799,#12013,#12014);
#9617=AXIS2_PLACEMENT_3D('',#14800,#12015,#12016);
#9618=AXIS2_PLACEMENT_3D('',#14801,#12017,#12018);
#9619=AXIS2_PLACEMENT_3D('',#14802,#12019,#12020);
#9620=AXIS2_PLACEMENT_3D('',#14803,#12021,#12022);
#9621=AXIS2_PLACEMENT_3D('',#14804,#12023,#12024);
#9622=AXIS2_PLACEMENT_3D('',#14805,#12025,#12026);
#9623=AXIS2_PLACEMENT_3D('',#14806,#12027,#12028);
#9624=AXIS2_PLACEMENT_3D('',#14807,#12029,#12030);
#9625=AXIS2_PLACEMENT_3D('',#14808,#12031,#12032);
#9626=AXIS2_PLACEMENT_3D('',#14809,#12033,#12034);
#9627=AXIS2_PLACEMENT_3D('',#14810,#12035,#12036);
#9628=AXIS2_PLACEMENT_3D('',#14811,#12037,#12038);
#9629=AXIS2_PLACEMENT_3D('',#14812,#12039,#12040);
#9630=AXIS2_PLACEMENT_3D('',#14813,#12041,#12042);
#9631=AXIS2_PLACEMENT_3D('',#14814,#12043,#12044);
#9632=AXIS2_PLACEMENT_3D('',#14815,#12045,#12046);
#9633=AXIS2_PLACEMENT_3D('',#14816,#12047,#12048);
#9634=AXIS2_PLACEMENT_3D('',#14817,#12049,#12050);
#9635=AXIS2_PLACEMENT_3D('',#14818,#12051,#12052);
#9636=AXIS2_PLACEMENT_3D('',#14820,#12053,#12054);
#9637=AXIS2_PLACEMENT_3D('',#14823,#12056,#12057);
#9638=AXIS2_PLACEMENT_3D('',#14824,#12058,#12059);
#9639=AXIS2_PLACEMENT_3D('',#14826,#12060,#12061);
#9640=AXIS2_PLACEMENT_3D('',#14829,#12063,#12064);
#9641=AXIS2_PLACEMENT_3D('',#14830,#12065,#12066);
#9642=AXIS2_PLACEMENT_3D('',#14835,#12068,#12069);
#9643=AXIS2_PLACEMENT_3D('',#14838,#12071,#12072);
#9644=AXIS2_PLACEMENT_3D('',#14839,#12073,#12074);
#9645=AXIS2_PLACEMENT_3D('',#14845,#12078,#12079);
#9646=AXIS2_PLACEMENT_3D('',#14848,#12081,#12082);
#9647=AXIS2_PLACEMENT_3D('',#14849,#12083,#12084);
#9648=AXIS2_PLACEMENT_3D('',#14853,#12087,#12088);
#9649=AXIS2_PLACEMENT_3D('',#14854,#12089,#12090);
#9650=AXIS2_PLACEMENT_3D('',#14855,#12091,#12092);
#9651=AXIS2_PLACEMENT_3D('',#14856,#12093,#12094);
#9652=AXIS2_PLACEMENT_3D('',#14857,#12095,#12096);
#9653=AXIS2_PLACEMENT_3D('',#14859,#12097,#12098);
#9654=AXIS2_PLACEMENT_3D('',#14862,#12100,#12101);
#9655=AXIS2_PLACEMENT_3D('',#14863,#12102,#12103);
#9656=AXIS2_PLACEMENT_3D('',#14865,#12104,#12105);
#9657=AXIS2_PLACEMENT_3D('',#14868,#12107,#12108);
#9658=AXIS2_PLACEMENT_3D('',#14869,#12109,#12110);
#9659=AXIS2_PLACEMENT_3D('',#14870,#12111,#12112);
#9660=AXIS2_PLACEMENT_3D('',#14871,#12113,#12114);
#9661=AXIS2_PLACEMENT_3D('',#14872,#12115,#12116);
#9662=AXIS2_PLACEMENT_3D('',#14874,#12117,#12118);
#9663=AXIS2_PLACEMENT_3D('',#14877,#12120,#12121);
#9664=AXIS2_PLACEMENT_3D('',#14878,#12122,#12123);
#9665=AXIS2_PLACEMENT_3D('',#14880,#12124,#12125);
#9666=AXIS2_PLACEMENT_3D('',#14883,#12127,#12128);
#9667=AXIS2_PLACEMENT_3D('',#14884,#12129,#12130);
#9668=AXIS2_PLACEMENT_3D('',#14885,#12131,#12132);
#9669=AXIS2_PLACEMENT_3D('',#14886,#12133,#12134);
#9670=AXIS2_PLACEMENT_3D('',#14887,#12135,#12136);
#9671=AXIS2_PLACEMENT_3D('',#14888,#12137,#12138);
#9672=AXIS2_PLACEMENT_3D('',#14889,#12139,#12140);
#9673=AXIS2_PLACEMENT_3D('',#14890,#12141,#12142);
#9674=AXIS2_PLACEMENT_3D('',#14891,#12143,#12144);
#9675=AXIS2_PLACEMENT_3D('',#14893,#12145,#12146);
#9676=AXIS2_PLACEMENT_3D('',#14896,#12148,#12149);
#9677=AXIS2_PLACEMENT_3D('',#14897,#12150,#12151);
#9678=AXIS2_PLACEMENT_3D('',#14898,#12152,#12153);
#9679=AXIS2_PLACEMENT_3D('',#14907,#12158,#12159);
#9680=AXIS2_PLACEMENT_3D('',#14917,#12165,#12166);
#9681=AXIS2_PLACEMENT_3D('',#14920,#12168,#12169);
#9682=AXIS2_PLACEMENT_3D('',#14921,#12170,#12171);
#9683=AXIS2_PLACEMENT_3D('',#14929,#12176,#12177);
#9684=AXIS2_PLACEMENT_3D('',#14935,#12181,#12182);
#9685=AXIS2_PLACEMENT_3D('',#14941,#12186,#12187);
#9686=AXIS2_PLACEMENT_3D('',#14942,#12188,#12189);
#9687=AXIS2_PLACEMENT_3D('',#14943,#12190,#12191);
#9688=AXIS2_PLACEMENT_3D('',#14945,#12192,#12193);
#9689=AXIS2_PLACEMENT_3D('',#14947,#12195,#12196);
#9690=AXIS2_PLACEMENT_3D('',#14948,#12197,#12198);
#9691=AXIS2_PLACEMENT_3D('',#14950,#12199,#12200);
#9692=AXIS2_PLACEMENT_3D('',#14951,#12201,#12202);
#9693=AXIS2_PLACEMENT_3D('',#14952,#12203,#12204);
#9694=AXIS2_PLACEMENT_3D('',#14955,#12206,#12207);
#9695=AXIS2_PLACEMENT_3D('',#14956,#12208,#12209);
#9696=AXIS2_PLACEMENT_3D('',#14957,#12210,#12211);
#9697=AXIS2_PLACEMENT_3D('',#14958,#12212,#12213);
#9698=AXIS2_PLACEMENT_3D('',#14962,#12215,#12216);
#9699=AXIS2_PLACEMENT_3D('',#14963,#12217,#12218);
#9700=AXIS2_PLACEMENT_3D('',#14976,#12219,#12220);
#9701=AXIS2_PLACEMENT_3D('',#14979,#12222,#12223);
#9702=AXIS2_PLACEMENT_3D('',#14981,#12224,#12225);
#9703=AXIS2_PLACEMENT_3D('',#14992,#12226,#12227);
#9704=AXIS2_PLACEMENT_3D('',#14994,#12229,#12230);
#9705=AXIS2_PLACEMENT_3D('',#14996,#12231,#12232);
#9706=AXIS2_PLACEMENT_3D('',#14999,#12234,#12235);
#9707=AXIS2_PLACEMENT_3D('',#15000,#12236,#12237);
#9708=AXIS2_PLACEMENT_3D('',#15009,#12242,#12243);
#9709=AXIS2_PLACEMENT_3D('',#15015,#12247,#12248);
#9710=AXIS2_PLACEMENT_3D('',#15019,#12251,#12252);
#9711=AXIS2_PLACEMENT_3D('',#15023,#12255,#12256);
#9712=AXIS2_PLACEMENT_3D('',#15025,#12258,#12259);
#9713=AXIS2_PLACEMENT_3D('',#15026,#12260,#12261);
#9714=AXIS2_PLACEMENT_3D('',#15027,#12262,#12263);
#9715=AXIS2_PLACEMENT_3D('',#15029,#12264,#12265);
#9716=AXIS2_PLACEMENT_3D('',#15031,#12266,#12267);
#9717=AXIS2_PLACEMENT_3D('',#15032,#12268,#12269);
#9718=AXIS2_PLACEMENT_3D('',#15035,#12271,#12272);
#9719=AXIS2_PLACEMENT_3D('',#15036,#12273,#12274);
#9720=AXIS2_PLACEMENT_3D('',#15037,#12275,#12276);
#9721=AXIS2_PLACEMENT_3D('',#15039,#12277,#12278);
#9722=AXIS2_PLACEMENT_3D('',#15041,#12280,#12281);
#9723=AXIS2_PLACEMENT_3D('',#15042,#12282,#12283);
#9724=AXIS2_PLACEMENT_3D('',#15043,#12284,#12285);
#9725=AXIS2_PLACEMENT_3D('',#15045,#12286,#12287);
#9726=AXIS2_PLACEMENT_3D('',#15048,#12289,#12290);
#9727=AXIS2_PLACEMENT_3D('',#15049,#12291,#12292);
#9728=AXIS2_PLACEMENT_3D('',#15050,#12293,#12294);
#9729=AXIS2_PLACEMENT_3D('',#15051,#12295,#12296);
#9730=AXIS2_PLACEMENT_3D('',#15052,#12297,#12298);
#9731=AXIS2_PLACEMENT_3D('',#15061,#12303,#12304);
#9732=AXIS2_PLACEMENT_3D('',#15067,#12308,#12309);
#9733=AXIS2_PLACEMENT_3D('',#15073,#12313,#12314);
#9734=AXIS2_PLACEMENT_3D('',#15079,#12318,#12319);
#9735=AXIS2_PLACEMENT_3D('',#15085,#12323,#12324);
#9736=AXIS2_PLACEMENT_3D('',#15088,#12327,#12328);
#9737=AXIS2_PLACEMENT_3D('',#15089,#12329,#12330);
#9738=AXIS2_PLACEMENT_3D('',#15091,#12331,#12332);
#9739=AXIS2_PLACEMENT_3D('',#15092,#12333,#12334);
#9740=AXIS2_PLACEMENT_3D('',#15094,#12335,#12336);
#9741=AXIS2_PLACEMENT_3D('',#15096,#12338,#12339);
#9742=AXIS2_PLACEMENT_3D('',#15098,#12340,#12341);
#9743=AXIS2_PLACEMENT_3D('',#15100,#12343,#12344);
#9744=AXIS2_PLACEMENT_3D('',#15102,#12345,#12346);
#9745=AXIS2_PLACEMENT_3D('',#15104,#12348,#12349);
#9746=AXIS2_PLACEMENT_3D('',#15105,#12350,#12351);
#9747=AXIS2_PLACEMENT_3D('',#15106,#12352,#12353);
#9748=AXIS2_PLACEMENT_3D('',#15107,#12354,#12355);
#9749=AXIS2_PLACEMENT_3D('',#15108,#12356,#12357);
#9750=AXIS2_PLACEMENT_3D('',#15109,#12358,#12359);
#9751=AXIS2_PLACEMENT_3D('',#15110,#12360,#12361);
#9752=AXIS2_PLACEMENT_3D('',#15111,#12362,#12363);
#9753=AXIS2_PLACEMENT_3D('',#15112,#12364,#12365);
#9754=DIRECTION('axis',(0.,0.,1.));
#9755=DIRECTION('refdir',(1.,0.,0.));
#9756=DIRECTION('axis',(0.,0.,1.));
#9757=DIRECTION('refdir',(1.,0.,0.));
#9758=DIRECTION('axis',(0.,0.,1.));
#9759=DIRECTION('refdir',(1.,0.,0.));
#9760=DIRECTION('center_axis',(0.,0.,1.));
#9761=DIRECTION('ref_axis',(1.,0.,0.));
#9762=DIRECTION('center_axis',(0.,0.,1.));
#9763=DIRECTION('ref_axis',(1.,0.,0.));
#9764=DIRECTION('',(0.,0.,1.));
#9765=DIRECTION('center_axis',(0.,0.,-1.));
#9766=DIRECTION('ref_axis',(1.,0.,0.));
#9767=DIRECTION('center_axis',(0.,0.,1.));
#9768=DIRECTION('ref_axis',(1.,0.,0.));
#9769=DIRECTION('center_axis',(0.,0.,1.));
#9770=DIRECTION('ref_axis',(1.,0.,0.));
#9771=DIRECTION('',(0.,0.,1.));
#9772=DIRECTION('center_axis',(0.,0.,-1.));
#9773=DIRECTION('ref_axis',(1.,0.,0.));
#9774=DIRECTION('center_axis',(0.,0.,1.));
#9775=DIRECTION('ref_axis',(1.,0.,0.));
#9776=DIRECTION('center_axis',(0.,0.,1.));
#9777=DIRECTION('ref_axis',(1.,0.,0.));
#9778=DIRECTION('',(0.,0.,1.));
#9779=DIRECTION('center_axis',(0.,0.,-1.));
#9780=DIRECTION('ref_axis',(1.,0.,0.));
#9781=DIRECTION('center_axis',(0.,0.,1.));
#9782=DIRECTION('ref_axis',(1.,0.,0.));
#9783=DIRECTION('center_axis',(0.,0.,1.));
#9784=DIRECTION('ref_axis',(1.,0.,0.));
#9785=DIRECTION('',(0.,0.,1.));
#9786=DIRECTION('center_axis',(0.,0.,-1.));
#9787=DIRECTION('ref_axis',(1.,0.,0.));
#9788=DIRECTION('center_axis',(0.,0.,1.));
#9789=DIRECTION('ref_axis',(1.,0.,0.));
#9790=DIRECTION('center_axis',(0.,0.,1.));
#9791=DIRECTION('ref_axis',(1.,0.,0.));
#9792=DIRECTION('',(0.,0.,1.));
#9793=DIRECTION('center_axis',(0.,0.,-1.));
#9794=DIRECTION('ref_axis',(1.,0.,0.));
#9795=DIRECTION('center_axis',(0.,0.,1.));
#9796=DIRECTION('ref_axis',(1.,0.,0.));
#9797=DIRECTION('center_axis',(0.,0.,1.));
#9798=DIRECTION('ref_axis',(1.,0.,0.));
#9799=DIRECTION('',(0.,0.,1.));
#9800=DIRECTION('center_axis',(0.,0.,-1.));
#9801=DIRECTION('ref_axis',(1.,0.,0.));
#9802=DIRECTION('center_axis',(0.,0.,1.));
#9803=DIRECTION('ref_axis',(1.,0.,0.));
#9804=DIRECTION('center_axis',(0.,0.,1.));
#9805=DIRECTION('ref_axis',(1.,0.,0.));
#9806=DIRECTION('',(0.,0.,1.));
#9807=DIRECTION('center_axis',(0.,0.,-1.));
#9808=DIRECTION('ref_axis',(1.,0.,0.));
#9809=DIRECTION('center_axis',(0.,0.,1.));
#9810=DIRECTION('ref_axis',(1.,0.,0.));
#9811=DIRECTION('center_axis',(0.,0.,1.));
#9812=DIRECTION('ref_axis',(1.,0.,0.));
#9813=DIRECTION('',(0.,0.,1.));
#9814=DIRECTION('center_axis',(0.,0.,-1.));
#9815=DIRECTION('ref_axis',(1.,0.,0.));
#9816=DIRECTION('center_axis',(0.,0.,1.));
#9817=DIRECTION('ref_axis',(1.,0.,0.));
#9818=DIRECTION('center_axis',(0.,0.,1.));
#9819=DIRECTION('ref_axis',(1.,0.,0.));
#9820=DIRECTION('',(0.,0.,1.));
#9821=DIRECTION('center_axis',(0.,0.,-1.));
#9822=DIRECTION('ref_axis',(1.,0.,0.));
#9823=DIRECTION('center_axis',(0.,0.,1.));
#9824=DIRECTION('ref_axis',(1.,0.,0.));
#9825=DIRECTION('center_axis',(0.,0.,1.));
#9826=DIRECTION('ref_axis',(1.,0.,0.));
#9827=DIRECTION('',(0.,0.,1.));
#9828=DIRECTION('center_axis',(0.,0.,-1.));
#9829=DIRECTION('ref_axis',(1.,0.,0.));
#9830=DIRECTION('center_axis',(0.,0.,1.));
#9831=DIRECTION('ref_axis',(1.,0.,0.));
#9832=DIRECTION('center_axis',(0.,0.,1.));
#9833=DIRECTION('ref_axis',(1.,0.,0.));
#9834=DIRECTION('',(0.,0.,1.));
#9835=DIRECTION('center_axis',(0.,0.,-1.));
#9836=DIRECTION('ref_axis',(1.,0.,0.));
#9837=DIRECTION('center_axis',(0.,0.,1.));
#9838=DIRECTION('ref_axis',(1.,0.,0.));
#9839=DIRECTION('center_axis',(0.,0.,1.));
#9840=DIRECTION('ref_axis',(1.,0.,0.));
#9841=DIRECTION('',(0.,0.,1.));
#9842=DIRECTION('center_axis',(0.,0.,-1.));
#9843=DIRECTION('ref_axis',(1.,0.,0.));
#9844=DIRECTION('center_axis',(0.,1.,0.));
#9845=DIRECTION('ref_axis',(-1.,0.,0.));
#9846=DIRECTION('',(-1.,0.,0.));
#9847=DIRECTION('',(0.,0.,1.));
#9848=DIRECTION('',(-1.,0.,0.));
#9849=DIRECTION('',(0.,0.,1.));
#9850=DIRECTION('center_axis',(1.,0.,0.));
#9851=DIRECTION('ref_axis',(0.,1.,0.));
#9852=DIRECTION('',(0.,1.,0.));
#9853=DIRECTION('',(0.,1.,0.));
#9854=DIRECTION('',(0.,0.,1.));
#9855=DIRECTION('center_axis',(0.,-1.,0.));
#9856=DIRECTION('ref_axis',(1.,0.,0.));
#9857=DIRECTION('',(1.,0.,0.));
#9858=DIRECTION('',(1.,0.,0.));
#9859=DIRECTION('',(0.,0.,1.));
#9860=DIRECTION('center_axis',(-1.,0.,0.));
#9861=DIRECTION('ref_axis',(0.,-1.,0.));
#9862=DIRECTION('',(0.,-1.,0.));
#9863=DIRECTION('',(0.,-1.,0.));
#9864=DIRECTION('center_axis',(0.,0.,1.));
#9865=DIRECTION('ref_axis',(1.,0.,0.));
#9866=DIRECTION('center_axis',(0.,0.,1.));
#9867=DIRECTION('ref_axis',(1.,0.,0.));
#9868=DIRECTION('axis',(0.,0.,1.));
#9869=DIRECTION('refdir',(1.,0.,0.));
#9870=DIRECTION('center_axis',(0.,0.,1.));
#9871=DIRECTION('ref_axis',(1.,0.,0.));
#9872=DIRECTION('center_axis',(0.,0.,1.));
#9873=DIRECTION('ref_axis',(1.,0.,0.));
#9874=DIRECTION('',(0.,0.,1.));
#9875=DIRECTION('center_axis',(0.,0.,-1.));
#9876=DIRECTION('ref_axis',(1.,0.,0.));
#9877=DIRECTION('center_axis',(0.,0.,1.));
#9878=DIRECTION('ref_axis',(1.,0.,0.));
#9879=DIRECTION('center_axis',(0.,0.,1.));
#9880=DIRECTION('ref_axis',(1.,0.,0.));
#9881=DIRECTION('',(0.,0.,1.));
#9882=DIRECTION('center_axis',(0.,0.,-1.));
#9883=DIRECTION('ref_axis',(1.,0.,0.));
#9884=DIRECTION('center_axis',(0.,0.,1.));
#9885=DIRECTION('ref_axis',(1.,0.,0.));
#9886=DIRECTION('center_axis',(0.,0.,1.));
#9887=DIRECTION('ref_axis',(1.,0.,0.));
#9888=DIRECTION('',(0.,0.,1.));
#9889=DIRECTION('center_axis',(0.,0.,-1.));
#9890=DIRECTION('ref_axis',(1.,0.,0.));
#9891=DIRECTION('center_axis',(0.,0.,1.));
#9892=DIRECTION('ref_axis',(1.,0.,0.));
#9893=DIRECTION('center_axis',(0.,0.,1.));
#9894=DIRECTION('ref_axis',(1.,0.,0.));
#9895=DIRECTION('',(0.,0.,1.));
#9896=DIRECTION('center_axis',(0.,0.,-1.));
#9897=DIRECTION('ref_axis',(1.,0.,0.));
#9898=DIRECTION('center_axis',(0.,1.,0.));
#9899=DIRECTION('ref_axis',(-1.,0.,0.));
#9900=DIRECTION('',(-1.,0.,0.));
#9901=DIRECTION('',(0.,0.,1.));
#9902=DIRECTION('',(-1.,0.,0.));
#9903=DIRECTION('',(0.,0.,1.));
#9904=DIRECTION('center_axis',(1.,0.,0.));
#9905=DIRECTION('ref_axis',(0.,1.,0.));
#9906=DIRECTION('',(0.,1.,0.));
#9907=DIRECTION('',(0.,1.,0.));
#9908=DIRECTION('',(0.,0.,1.));
#9909=DIRECTION('center_axis',(0.,-1.,0.));
#9910=DIRECTION('ref_axis',(1.,0.,0.));
#9911=DIRECTION('',(1.,0.,0.));
#9912=DIRECTION('',(1.,0.,0.));
#9913=DIRECTION('',(0.,0.,1.));
#9914=DIRECTION('center_axis',(-1.,0.,0.));
#9915=DIRECTION('ref_axis',(0.,-1.,0.));
#9916=DIRECTION('',(0.,-1.,0.));
#9917=DIRECTION('',(0.,-1.,0.));
#9918=DIRECTION('center_axis',(0.,0.,1.));
#9919=DIRECTION('ref_axis',(1.,0.,0.));
#9920=DIRECTION('center_axis',(0.,0.,1.));
#9921=DIRECTION('ref_axis',(1.,0.,0.));
#9922=DIRECTION('axis',(0.,0.,1.));
#9923=DIRECTION('refdir',(1.,0.,0.));
#9924=DIRECTION('center_axis',(0.,1.,0.));
#9925=DIRECTION('ref_axis',(-1.,0.,0.));
#9926=DIRECTION('',(-1.,0.,0.));
#9927=DIRECTION('',(0.,0.,1.));
#9928=DIRECTION('',(-1.,0.,0.));
#9929=DIRECTION('',(0.,0.,1.));
#9930=DIRECTION('center_axis',(1.,0.,0.));
#9931=DIRECTION('ref_axis',(0.,1.,0.));
#9932=DIRECTION('',(0.,1.,0.));
#9933=DIRECTION('',(0.,1.,0.));
#9934=DIRECTION('',(0.,0.,1.));
#9935=DIRECTION('center_axis',(0.,-1.,0.));
#9936=DIRECTION('ref_axis',(1.,0.,0.));
#9937=DIRECTION('',(1.,0.,0.));
#9938=DIRECTION('',(1.,0.,0.));
#9939=DIRECTION('',(0.,0.,1.));
#9940=DIRECTION('center_axis',(-1.,0.,0.));
#9941=DIRECTION('ref_axis',(0.,-1.,0.));
#9942=DIRECTION('',(0.,-1.,0.));
#9943=DIRECTION('',(0.,-1.,0.));
#9944=DIRECTION('center_axis',(0.,0.,1.));
#9945=DIRECTION('ref_axis',(1.,0.,0.));
#9946=DIRECTION('center_axis',(0.,0.,1.));
#9947=DIRECTION('ref_axis',(1.,0.,0.));
#9948=DIRECTION('axis',(0.,0.,1.));
#9949=DIRECTION('refdir',(1.,0.,0.));
#9950=DIRECTION('center_axis',(0.,1.,0.));
#9951=DIRECTION('ref_axis',(-1.,0.,0.));
#9952=DIRECTION('',(-1.,0.,0.));
#9953=DIRECTION('',(0.,0.,1.));
#9954=DIRECTION('',(-1.,0.,0.));
#9955=DIRECTION('',(0.,0.,1.));
#9956=DIRECTION('center_axis',(1.,0.,0.));
#9957=DIRECTION('ref_axis',(0.,1.,0.));
#9958=DIRECTION('',(0.,1.,0.));
#9959=DIRECTION('',(0.,1.,0.));
#9960=DIRECTION('',(0.,0.,1.));
#9961=DIRECTION('center_axis',(0.,-1.,0.));
#9962=DIRECTION('ref_axis',(1.,0.,0.));
#9963=DIRECTION('',(1.,0.,0.));
#9964=DIRECTION('',(1.,0.,0.));
#9965=DIRECTION('',(0.,0.,1.));
#9966=DIRECTION('center_axis',(-1.,0.,0.));
#9967=DIRECTION('ref_axis',(0.,-1.,0.));
#9968=DIRECTION('',(0.,-1.,0.));
#9969=DIRECTION('',(0.,-1.,0.));
#9970=DIRECTION('center_axis',(0.,0.,1.));
#9971=DIRECTION('ref_axis',(1.,0.,0.));
#9972=DIRECTION('center_axis',(0.,0.,1.));
#9973=DIRECTION('ref_axis',(1.,0.,0.));
#9974=DIRECTION('axis',(0.,0.,1.));
#9975=DIRECTION('refdir',(1.,0.,0.));
#9976=DIRECTION('center_axis',(0.,1.,0.));
#9977=DIRECTION('ref_axis',(1.,0.,0.));
#9978=DIRECTION('center_axis',(0.,1.,0.));
#9979=DIRECTION('ref_axis',(1.,0.,0.));
#9980=DIRECTION('',(0.,1.,0.));
#9981=DIRECTION('center_axis',(0.,-1.,0.));
#9982=DIRECTION('ref_axis',(1.,0.,0.));
#9983=DIRECTION('center_axis',(0.,0.,1.));
#9984=DIRECTION('ref_axis',(1.,0.,0.));
#9985=DIRECTION('center_axis',(0.,0.,1.));
#9986=DIRECTION('ref_axis',(1.,0.,0.));
#9987=DIRECTION('',(0.,0.,1.));
#9988=DIRECTION('center_axis',(0.,0.,-1.));
#9989=DIRECTION('ref_axis',(1.,0.,0.));
#9990=DIRECTION('center_axis',(0.,0.,1.));
#9991=DIRECTION('ref_axis',(1.,0.,0.));
#9992=DIRECTION('center_axis',(0.,0.,1.));
#9993=DIRECTION('ref_axis',(1.,0.,0.));
#9994=DIRECTION('center_axis',(0.,0.,1.));
#9995=DIRECTION('ref_axis',(1.,0.,0.));
#9996=DIRECTION('',(0.,0.,1.));
#9997=DIRECTION('center_axis',(0.,0.,-1.));
#9998=DIRECTION('ref_axis',(1.,0.,0.));
#9999=DIRECTION('center_axis',(0.,0.,1.));
#10000=DIRECTION('ref_axis',(1.,0.,0.));
#10001=DIRECTION('center_axis',(0.,0.,1.));
#10002=DIRECTION('ref_axis',(1.,0.,0.));
#10003=DIRECTION('center_axis',(0.,0.,1.));
#10004=DIRECTION('ref_axis',(1.,0.,0.));
#10005=DIRECTION('',(0.,0.,1.));
#10006=DIRECTION('center_axis',(0.,0.,-1.));
#10007=DIRECTION('ref_axis',(1.,0.,0.));
#10008=DIRECTION('center_axis',(0.,0.,1.));
#10009=DIRECTION('ref_axis',(1.,0.,0.));
#10010=DIRECTION('center_axis',(0.,0.,1.));
#10011=DIRECTION('ref_axis',(1.,0.,0.));
#10012=DIRECTION('center_axis',(0.,0.,1.));
#10013=DIRECTION('ref_axis',(1.,0.,0.));
#10014=DIRECTION('',(0.,0.,1.));
#10015=DIRECTION('center_axis',(0.,0.,-1.));
#10016=DIRECTION('ref_axis',(1.,0.,0.));
#10017=DIRECTION('center_axis',(0.,0.,1.));
#10018=DIRECTION('ref_axis',(1.,0.,0.));
#10019=DIRECTION('center_axis',(0.,1.,0.));
#10020=DIRECTION('ref_axis',(1.,0.,0.));
#10021=DIRECTION('center_axis',(0.,1.,0.));
#10022=DIRECTION('ref_axis',(1.,0.,0.));
#10023=DIRECTION('',(0.,1.,0.));
#10024=DIRECTION('center_axis',(0.,-1.,0.));
#10025=DIRECTION('ref_axis',(1.,0.,0.));
#10026=DIRECTION('center_axis',(0.,1.,0.));
#10027=DIRECTION('ref_axis',(1.,0.,0.));
#10028=DIRECTION('center_axis',(0.,1.,0.));
#10029=DIRECTION('ref_axis',(1.,0.,0.));
#10030=DIRECTION('',(0.,1.,0.));
#10031=DIRECTION('center_axis',(0.,-1.,0.));
#10032=DIRECTION('ref_axis',(1.,0.,0.));
#10033=DIRECTION('center_axis',(0.,1.,0.));
#10034=DIRECTION('ref_axis',(1.,0.,0.));
#10035=DIRECTION('center_axis',(0.,1.,0.));
#10036=DIRECTION('ref_axis',(1.,0.,0.));
#10037=DIRECTION('',(0.,1.,0.));
#10038=DIRECTION('center_axis',(0.,-1.,0.));
#10039=DIRECTION('ref_axis',(1.,0.,0.));
#10040=DIRECTION('center_axis',(0.,1.,0.));
#10041=DIRECTION('ref_axis',(1.,0.,0.));
#10042=DIRECTION('center_axis',(0.,1.,0.));
#10043=DIRECTION('ref_axis',(1.,0.,0.));
#10044=DIRECTION('',(0.,1.,0.));
#10045=DIRECTION('center_axis',(0.,-1.,0.));
#10046=DIRECTION('ref_axis',(1.,0.,0.));
#10047=DIRECTION('center_axis',(0.,0.,1.));
#10048=DIRECTION('ref_axis',(1.,0.,0.));
#10049=DIRECTION('center_axis',(0.,0.,1.));
#10050=DIRECTION('ref_axis',(1.,0.,0.));
#10051=DIRECTION('',(0.,0.,1.));
#10052=DIRECTION('center_axis',(0.,0.,-1.));
#10053=DIRECTION('ref_axis',(1.,0.,0.));
#10054=DIRECTION('center_axis',(0.,0.,1.));
#10055=DIRECTION('ref_axis',(1.,0.,0.));
#10056=DIRECTION('center_axis',(0.,0.,1.));
#10057=DIRECTION('ref_axis',(1.,0.,0.));
#10058=DIRECTION('',(0.,0.,1.));
#10059=DIRECTION('center_axis',(0.,0.,-1.));
#10060=DIRECTION('ref_axis',(1.,0.,0.));
#10061=DIRECTION('center_axis',(0.,0.,1.));
#10062=DIRECTION('ref_axis',(1.,0.,0.));
#10063=DIRECTION('center_axis',(0.,0.,1.));
#10064=DIRECTION('ref_axis',(1.,0.,0.));
#10065=DIRECTION('',(0.,0.,1.));
#10066=DIRECTION('center_axis',(0.,0.,-1.));
#10067=DIRECTION('ref_axis',(1.,0.,0.));
#10068=DIRECTION('center_axis',(0.,0.,1.));
#10069=DIRECTION('ref_axis',(1.,0.,0.));
#10070=DIRECTION('center_axis',(0.,0.,1.));
#10071=DIRECTION('ref_axis',(1.,0.,0.));
#10072=DIRECTION('',(0.,0.,1.));
#10073=DIRECTION('center_axis',(0.,0.,-1.));
#10074=DIRECTION('ref_axis',(1.,0.,0.));
#10075=DIRECTION('center_axis',(0.,0.,1.));
#10076=DIRECTION('ref_axis',(1.,0.,0.));
#10077=DIRECTION('center_axis',(0.,0.,1.));
#10078=DIRECTION('ref_axis',(1.,0.,0.));
#10079=DIRECTION('',(0.,0.,1.));
#10080=DIRECTION('center_axis',(0.,0.,-1.));
#10081=DIRECTION('ref_axis',(1.,0.,0.));
#10082=DIRECTION('center_axis',(0.,0.,1.));
#10083=DIRECTION('ref_axis',(1.,0.,0.));
#10084=DIRECTION('center_axis',(0.,0.,1.));
#10085=DIRECTION('ref_axis',(1.,0.,0.));
#10086=DIRECTION('center_axis',(0.,0.,1.));
#10087=DIRECTION('ref_axis',(1.,0.,0.));
#10088=DIRECTION('center_axis',(0.,0.,1.));
#10089=DIRECTION('ref_axis',(1.,0.,0.));
#10090=DIRECTION('',(0.,0.,1.));
#10091=DIRECTION('center_axis',(0.,1.,0.));
#10092=DIRECTION('ref_axis',(1.,0.,0.));
#10093=DIRECTION('center_axis',(0.,1.,0.));
#10094=DIRECTION('ref_axis',(1.,0.,0.));
#10095=DIRECTION('',(0.,1.,0.));
#10096=DIRECTION('center_axis',(0.,-1.,0.));
#10097=DIRECTION('ref_axis',(1.,0.,0.));
#10098=DIRECTION('center_axis',(0.,0.,1.));
#10099=DIRECTION('ref_axis',(1.,0.,0.));
#10100=DIRECTION('',(0.,0.,1.));
#10101=DIRECTION('center_axis',(0.,0.,1.));
#10102=DIRECTION('ref_axis',(1.,0.,0.));
#10103=DIRECTION('',(0.,0.,-1.));
#10104=DIRECTION('center_axis',(0.,0.,1.));
#10105=DIRECTION('ref_axis',(1.,0.,0.));
#10106=DIRECTION('center_axis',(0.,-1.,0.));
#10107=DIRECTION('ref_axis',(1.,0.,0.));
#10108=DIRECTION('',(-1.,0.,0.));
#10109=DIRECTION('',(0.,0.,1.));
#10110=DIRECTION('',(1.,0.,0.));
#10111=DIRECTION('',(0.,0.,1.));
#10112=DIRECTION('',(1.,0.,0.));
#10113=DIRECTION('',(0.,0.,1.));
#10114=DIRECTION('',(1.,0.,0.));
#10115=DIRECTION('center_axis',(0.,1.,0.));
#10116=DIRECTION('ref_axis',(1.,0.,0.));
#10117=DIRECTION('',(1.,0.,0.));
#10118=DIRECTION('center_axis',(0.,0.,1.));
#10119=DIRECTION('ref_axis',(1.,0.,0.));
#10120=DIRECTION('',(1.,0.,0.));
#10121=DIRECTION('',(0.,1.,0.));
#10122=DIRECTION('center_axis',(0.,0.,1.));
#10123=DIRECTION('ref_axis',(1.,0.,0.));
#10124=DIRECTION('',(0.,-1.,0.));
#10125=DIRECTION('',(1.,0.,0.));
#10126=DIRECTION('',(0.,1.,0.));
#10127=DIRECTION('',(-1.,0.,0.));
#10128=DIRECTION('',(-1.,0.,0.));
#10129=DIRECTION('',(0.,1.,0.));
#10130=DIRECTION('',(0.,-1.,0.));
#10131=DIRECTION('center_axis',(0.,1.,0.));
#10132=DIRECTION('ref_axis',(-1.,0.,0.));
#10133=DIRECTION('',(-1.,0.,0.));
#10134=DIRECTION('',(0.,0.,1.));
#10135=DIRECTION('',(0.,0.,1.));
#10136=DIRECTION('center_axis',(1.,0.,0.));
#10137=DIRECTION('ref_axis',(0.,1.,0.));
#10138=DIRECTION('',(0.,1.,0.));
#10139=DIRECTION('',(0.,0.,1.));
#10140=DIRECTION('center_axis',(0.,-1.,0.));
#10141=DIRECTION('ref_axis',(1.,0.,0.));
#10142=DIRECTION('',(1.,0.,0.));
#10143=DIRECTION('',(0.,0.,1.));
#10144=DIRECTION('center_axis',(-1.,0.,0.));
#10145=DIRECTION('ref_axis',(0.,-1.,0.));
#10146=DIRECTION('',(0.,-1.,0.));
#10147=DIRECTION('center_axis',(1.,0.,0.));
#10148=DIRECTION('ref_axis',(0.,1.,0.));
#10149=DIRECTION('',(0.,0.,1.));
#10150=DIRECTION('',(0.,-1.,0.));
#10151=DIRECTION('center_axis',(0.,1.,0.));
#10152=DIRECTION('ref_axis',(6.12323399573677E-17,0.,-1.));
#10153=DIRECTION('',(0.,1.,0.));
#10154=DIRECTION('',(0.,-1.,0.));
#10155=DIRECTION('center_axis',(0.,1.,0.));
#10156=DIRECTION('ref_axis',(1.,0.,0.));
#10157=DIRECTION('center_axis',(0.,1.,0.));
#10158=DIRECTION('ref_axis',(-1.,0.,0.));
#10159=DIRECTION('',(-1.,0.,0.));
#10160=DIRECTION('',(-1.,0.,0.));
#10161=DIRECTION('',(0.,0.,1.));
#10162=DIRECTION('',(-1.,0.,0.));
#10163=DIRECTION('',(0.,0.,1.));
#10164=DIRECTION('center_axis',(0.,0.,-1.));
#10165=DIRECTION('ref_axis',(-1.,0.,0.));
#10166=DIRECTION('center_axis',(0.,0.,-1.));
#10167=DIRECTION('ref_axis',(-1.,0.,0.));
#10168=DIRECTION('center_axis',(1.,0.,0.));
#10169=DIRECTION('ref_axis',(0.,1.,0.));
#10170=DIRECTION('',(0.,1.,0.));
#10171=DIRECTION('center_axis',(-1.,0.,0.));
#10172=DIRECTION('ref_axis',(0.,-1.,0.));
#10173=DIRECTION('',(0.,-1.,0.));
#10174=DIRECTION('center_axis',(0.,0.,1.));
#10175=DIRECTION('ref_axis',(1.,0.,0.));
#10176=DIRECTION('center_axis',(0.,0.,1.));
#10177=DIRECTION('ref_axis',(1.,0.,0.));
#10178=DIRECTION('axis',(0.,0.,1.));
#10179=DIRECTION('refdir',(1.,0.,0.));
#10180=DIRECTION('center_axis',(0.,1.,0.));
#10181=DIRECTION('ref_axis',(1.,0.,0.));
#10182=DIRECTION('center_axis',(0.,1.,0.));
#10183=DIRECTION('ref_axis',(1.,0.,0.));
#10184=DIRECTION('',(0.,1.,0.));
#10185=DIRECTION('center_axis',(0.,-1.,0.));
#10186=DIRECTION('ref_axis',(1.,0.,0.));
#10187=DIRECTION('center_axis',(0.,1.,0.));
#10188=DIRECTION('ref_axis',(1.,0.,0.));
#10189=DIRECTION('center_axis',(0.,1.,0.));
#10190=DIRECTION('ref_axis',(1.,0.,0.));
#10191=DIRECTION('',(0.,1.,0.));
#10192=DIRECTION('center_axis',(0.,-1.,0.));
#10193=DIRECTION('ref_axis',(1.,0.,0.));
#10194=DIRECTION('center_axis',(0.,1.,0.));
#10195=DIRECTION('ref_axis',(1.,0.,0.));
#10196=DIRECTION('center_axis',(0.,1.,0.));
#10197=DIRECTION('ref_axis',(1.,0.,0.));
#10198=DIRECTION('',(0.,1.,0.));
#10199=DIRECTION('center_axis',(0.,-1.,0.));
#10200=DIRECTION('ref_axis',(1.,0.,0.));
#10201=DIRECTION('center_axis',(0.,1.,0.));
#10202=DIRECTION('ref_axis',(1.,0.,0.));
#10203=DIRECTION('center_axis',(0.,1.,0.));
#10204=DIRECTION('ref_axis',(1.,0.,0.));
#10205=DIRECTION('',(0.,1.,0.));
#10206=DIRECTION('center_axis',(0.,-1.,0.));
#10207=DIRECTION('ref_axis',(1.,0.,0.));
#10208=DIRECTION('center_axis',(0.,1.,0.));
#10209=DIRECTION('ref_axis',(1.,0.,0.));
#10210=DIRECTION('center_axis',(0.,1.,0.));
#10211=DIRECTION('ref_axis',(1.,0.,0.));
#10212=DIRECTION('',(0.,-1.,0.));
#10213=DIRECTION('center_axis',(0.,-1.,0.));
#10214=DIRECTION('ref_axis',(1.,0.,0.));
#10215=DIRECTION('center_axis',(0.,1.,0.));
#10216=DIRECTION('ref_axis',(1.,0.,0.));
#10217=DIRECTION('center_axis',(0.,-1.,0.));
#10218=DIRECTION('ref_axis',(1.,0.,0.));
#10219=DIRECTION('center_axis',(0.,1.,0.));
#10220=DIRECTION('ref_axis',(1.,0.,0.));
#10221=DIRECTION('',(0.,-1.,0.));
#10222=DIRECTION('center_axis',(0.,-1.,0.));
#10223=DIRECTION('ref_axis',(1.,0.,0.));
#10224=DIRECTION('center_axis',(0.,1.,0.));
#10225=DIRECTION('ref_axis',(1.,0.,0.));
#10226=DIRECTION('center_axis',(0.,1.,0.));
#10227=DIRECTION('ref_axis',(1.,0.,0.));
#10228=DIRECTION('',(0.,-1.,0.));
#10229=DIRECTION('center_axis',(0.,1.,0.));
#10230=DIRECTION('ref_axis',(1.,0.,0.));
#10231=DIRECTION('center_axis',(0.,1.,0.));
#10232=DIRECTION('ref_axis',(1.,0.,0.));
#10233=DIRECTION('center_axis',(0.,1.,0.));
#10234=DIRECTION('ref_axis',(1.,0.,0.));
#10235=DIRECTION('axis',(0.,0.,1.));
#10236=DIRECTION('refdir',(1.,0.,0.));
#10237=DIRECTION('center_axis',(0.,1.,0.));
#10238=DIRECTION('ref_axis',(1.,0.,0.));
#10239=DIRECTION('center_axis',(0.,1.,0.));
#10240=DIRECTION('ref_axis',(1.,0.,0.));
#10241=DIRECTION('',(0.,1.,0.));
#10242=DIRECTION('center_axis',(0.,-1.,0.));
#10243=DIRECTION('ref_axis',(1.,0.,0.));
#10244=DIRECTION('center_axis',(0.,1.,0.));
#10245=DIRECTION('ref_axis',(1.,0.,0.));
#10246=DIRECTION('center_axis',(0.,1.,0.));
#10247=DIRECTION('ref_axis',(1.,0.,0.));
#10248=DIRECTION('',(0.,1.,0.));
#10249=DIRECTION('center_axis',(0.,-1.,0.));
#10250=DIRECTION('ref_axis',(1.,0.,0.));
#10251=DIRECTION('center_axis',(0.,1.,0.));
#10252=DIRECTION('ref_axis',(1.,0.,0.));
#10253=DIRECTION('center_axis',(0.,1.,0.));
#10254=DIRECTION('ref_axis',(1.,0.,0.));
#10255=DIRECTION('',(0.,1.,0.));
#10256=DIRECTION('center_axis',(0.,-1.,0.));
#10257=DIRECTION('ref_axis',(1.,0.,0.));
#10258=DIRECTION('center_axis',(0.,1.,0.));
#10259=DIRECTION('ref_axis',(1.,0.,0.));
#10260=DIRECTION('center_axis',(0.,1.,0.));
#10261=DIRECTION('ref_axis',(1.,0.,0.));
#10262=DIRECTION('',(0.,1.,0.));
#10263=DIRECTION('center_axis',(0.,-1.,0.));
#10264=DIRECTION('ref_axis',(1.,0.,0.));
#10265=DIRECTION('center_axis',(0.,1.,0.));
#10266=DIRECTION('ref_axis',(1.,0.,0.));
#10267=DIRECTION('center_axis',(0.,1.,0.));
#10268=DIRECTION('ref_axis',(1.,0.,0.));
#10269=DIRECTION('',(0.,-1.,0.));
#10270=DIRECTION('center_axis',(0.,1.,0.));
#10271=DIRECTION('ref_axis',(1.,0.,0.));
#10272=DIRECTION('center_axis',(0.,1.,0.));
#10273=DIRECTION('ref_axis',(1.,0.,0.));
#10274=DIRECTION('center_axis',(0.,-1.,0.));
#10275=DIRECTION('ref_axis',(1.,0.,0.));
#10276=DIRECTION('center_axis',(0.,1.,0.));
#10277=DIRECTION('ref_axis',(1.,0.,0.));
#10278=DIRECTION('center_axis',(0.,-1.,0.));
#10279=DIRECTION('ref_axis',(1.,0.,0.));
#10280=DIRECTION('',(0.,-1.,0.));
#10281=DIRECTION('center_axis',(0.,1.,0.));
#10282=DIRECTION('ref_axis',(1.,0.,0.));
#10283=DIRECTION('center_axis',(0.,1.,0.));
#10284=DIRECTION('ref_axis',(1.,0.,0.));
#10285=DIRECTION('',(0.,-1.,0.));
#10286=DIRECTION('center_axis',(0.,1.,0.));
#10287=DIRECTION('ref_axis',(1.,0.,0.));
#10288=DIRECTION('center_axis',(0.,1.,0.));
#10289=DIRECTION('ref_axis',(1.,0.,0.));
#10290=DIRECTION('center_axis',(0.,1.,0.));
#10291=DIRECTION('ref_axis',(1.,0.,0.));
#10292=DIRECTION('axis',(0.,0.,1.));
#10293=DIRECTION('refdir',(1.,0.,0.));
#10294=DIRECTION('center_axis',(0.,0.,1.));
#10295=DIRECTION('ref_axis',(1.,0.,0.));
#10296=DIRECTION('center_axis',(0.,0.,1.));
#10297=DIRECTION('ref_axis',(1.,0.,0.));
#10298=DIRECTION('',(0.,0.,1.));
#10299=DIRECTION('center_axis',(0.,0.,-1.));
#10300=DIRECTION('ref_axis',(1.,0.,0.));
#10301=DIRECTION('center_axis',(0.,0.,1.));
#10302=DIRECTION('ref_axis',(1.,0.,0.));
#10303=DIRECTION('center_axis',(0.,0.,1.));
#10304=DIRECTION('ref_axis',(1.,0.,0.));
#10305=DIRECTION('center_axis',(0.,0.,1.));
#10306=DIRECTION('ref_axis',(1.,0.,0.));
#10307=DIRECTION('center_axis',(0.,0.,1.));
#10308=DIRECTION('ref_axis',(1.,0.,0.));
#10309=DIRECTION('',(0.,0.,1.));
#10310=DIRECTION('center_axis',(0.,0.,-1.));
#10311=DIRECTION('ref_axis',(1.,0.,0.));
#10312=DIRECTION('center_axis',(0.,0.,1.));
#10313=DIRECTION('ref_axis',(1.,0.,0.));
#10314=DIRECTION('center_axis',(0.,0.,1.));
#10315=DIRECTION('ref_axis',(1.,0.,0.));
#10316=DIRECTION('center_axis',(0.,0.,1.));
#10317=DIRECTION('ref_axis',(1.,0.,0.));
#10318=DIRECTION('center_axis',(0.,0.,1.));
#10319=DIRECTION('ref_axis',(1.,0.,0.));
#10320=DIRECTION('',(0.,0.,1.));
#10321=DIRECTION('center_axis',(0.,0.,-1.));
#10322=DIRECTION('ref_axis',(1.,0.,0.));
#10323=DIRECTION('center_axis',(0.,0.,1.));
#10324=DIRECTION('ref_axis',(1.,0.,0.));
#10325=DIRECTION('center_axis',(0.,0.,1.));
#10326=DIRECTION('ref_axis',(1.,0.,0.));
#10327=DIRECTION('center_axis',(0.,0.,1.));
#10328=DIRECTION('ref_axis',(1.,0.,0.));
#10329=DIRECTION('center_axis',(0.,0.,1.));
#10330=DIRECTION('ref_axis',(1.,0.,0.));
#10331=DIRECTION('',(0.,0.,1.));
#10332=DIRECTION('center_axis',(0.,0.,-1.));
#10333=DIRECTION('ref_axis',(1.,0.,0.));
#10334=DIRECTION('center_axis',(0.,0.,1.));
#10335=DIRECTION('ref_axis',(1.,0.,0.));
#10336=DIRECTION('center_axis',(0.,0.,1.));
#10337=DIRECTION('ref_axis',(1.,0.,0.));
#10338=DIRECTION('center_axis',(0.,0.,1.));
#10339=DIRECTION('ref_axis',(1.,0.,0.));
#10340=DIRECTION('center_axis',(0.,0.,1.));
#10341=DIRECTION('ref_axis',(1.,0.,0.));
#10342=DIRECTION('',(0.,0.,1.));
#10343=DIRECTION('center_axis',(0.,0.,1.));
#10344=DIRECTION('ref_axis',(1.,0.,0.));
#10345=DIRECTION('center_axis',(0.,0.,1.));
#10346=DIRECTION('ref_axis',(1.,0.,0.));
#10347=DIRECTION('',(0.,0.,1.));
#10348=DIRECTION('center_axis',(0.,0.,1.));
#10349=DIRECTION('ref_axis',(1.,0.,0.));
#10350=DIRECTION('center_axis',(0.,0.,1.));
#10351=DIRECTION('ref_axis',(1.,0.,0.));
#10352=DIRECTION('',(0.,0.,1.));
#10353=DIRECTION('center_axis',(0.,0.,1.));
#10354=DIRECTION('ref_axis',(1.,0.,0.));
#10355=DIRECTION('center_axis',(0.,0.,1.));
#10356=DIRECTION('ref_axis',(1.,0.,0.));
#10357=DIRECTION('',(0.,0.,1.));
#10358=DIRECTION('center_axis',(0.,0.,1.));
#10359=DIRECTION('ref_axis',(1.,0.,0.));
#10360=DIRECTION('center_axis',(0.,0.,1.));
#10361=DIRECTION('ref_axis',(1.,0.,0.));
#10362=DIRECTION('',(0.,0.,-1.));
#10363=DIRECTION('center_axis',(0.,0.,1.));
#10364=DIRECTION('ref_axis',(1.,0.,0.));
#10365=DIRECTION('center_axis',(0.,0.,1.));
#10366=DIRECTION('ref_axis',(1.,0.,0.));
#10367=DIRECTION('center_axis',(0.,0.,-1.));
#10368=DIRECTION('ref_axis',(1.,0.,0.));
#10369=DIRECTION('center_axis',(0.,0.,1.));
#10370=DIRECTION('ref_axis',(1.,0.,0.));
#10371=DIRECTION('center_axis',(0.,0.,-1.));
#10372=DIRECTION('ref_axis',(1.,0.,0.));
#10373=DIRECTION('',(0.,0.,-1.));
#10374=DIRECTION('center_axis',(0.,0.,1.));
#10375=DIRECTION('ref_axis',(1.,0.,0.));
#10376=DIRECTION('center_axis',(0.,0.,1.));
#10377=DIRECTION('ref_axis',(1.,0.,0.));
#10378=DIRECTION('',(0.,0.,-1.));
#10379=DIRECTION('center_axis',(0.,0.,1.));
#10380=DIRECTION('ref_axis',(1.,0.,0.));
#10381=DIRECTION('center_axis',(0.,0.,1.));
#10382=DIRECTION('ref_axis',(1.,0.,0.));
#10383=DIRECTION('center_axis',(0.,0.,1.));
#10384=DIRECTION('ref_axis',(1.,0.,0.));
#10385=DIRECTION('axis',(0.,0.,1.));
#10386=DIRECTION('refdir',(1.,0.,0.));
#10387=DIRECTION('center_axis',(0.,1.,0.));
#10388=DIRECTION('ref_axis',(-1.,0.,0.));
#10389=DIRECTION('',(-1.,0.,0.));
#10390=DIRECTION('',(0.,0.,1.));
#10391=DIRECTION('',(-1.,0.,0.));
#10392=DIRECTION('',(0.,0.,1.));
#10393=DIRECTION('center_axis',(1.,0.,0.));
#10394=DIRECTION('ref_axis',(0.,1.,0.));
#10395=DIRECTION('',(0.,1.,0.));
#10396=DIRECTION('',(0.,1.,0.));
#10397=DIRECTION('',(0.,0.,1.));
#10398=DIRECTION('center_axis',(0.,-1.,0.));
#10399=DIRECTION('ref_axis',(1.,0.,0.));
#10400=DIRECTION('',(1.,0.,0.));
#10401=DIRECTION('',(1.,0.,0.));
#10402=DIRECTION('',(0.,0.,1.));
#10403=DIRECTION('center_axis',(-1.,0.,0.));
#10404=DIRECTION('ref_axis',(0.,-1.,0.));
#10405=DIRECTION('',(0.,-1.,0.));
#10406=DIRECTION('',(0.,-1.,0.));
#10407=DIRECTION('center_axis',(0.,0.,1.));
#10408=DIRECTION('ref_axis',(1.,0.,0.));
#10409=DIRECTION('center_axis',(0.,0.,1.));
#10410=DIRECTION('ref_axis',(1.,0.,0.));
#10411=DIRECTION('axis',(0.,0.,1.));
#10412=DIRECTION('refdir',(1.,0.,0.));
#10413=DIRECTION('center_axis',(0.,0.,1.));
#10414=DIRECTION('ref_axis',(1.,0.,0.));
#10415=DIRECTION('center_axis',(0.,0.,1.));
#10416=DIRECTION('ref_axis',(1.,0.,0.));
#10417=DIRECTION('',(0.,0.,1.));
#10418=DIRECTION('center_axis',(0.,0.,1.));
#10419=DIRECTION('ref_axis',(1.,0.,0.));
#10420=DIRECTION('center_axis',(0.,0.,1.));
#10421=DIRECTION('ref_axis',(1.,0.,0.));
#10422=DIRECTION('center_axis',(0.,0.,1.));
#10423=DIRECTION('ref_axis',(1.,0.,0.));
#10424=DIRECTION('center_axis',(0.,0.,1.));
#10425=DIRECTION('ref_axis',(1.,0.,0.));
#10426=DIRECTION('',(0.,0.,1.));
#10427=DIRECTION('center_axis',(0.,0.,1.));
#10428=DIRECTION('ref_axis',(1.,0.,0.));
#10429=DIRECTION('center_axis',(0.,0.,1.));
#10430=DIRECTION('ref_axis',(1.,0.,0.));
#10431=DIRECTION('center_axis',(0.,1.,0.));
#10432=DIRECTION('ref_axis',(-1.,0.,0.));
#10433=DIRECTION('',(-1.,0.,0.));
#10434=DIRECTION('',(0.,0.,1.));
#10435=DIRECTION('',(-1.,0.,0.));
#10436=DIRECTION('',(0.,0.,1.));
#10437=DIRECTION('center_axis',(1.,0.,0.));
#10438=DIRECTION('ref_axis',(0.,1.,0.));
#10439=DIRECTION('',(0.,1.,0.));
#10440=DIRECTION('',(0.,1.,0.));
#10441=DIRECTION('',(0.,0.,1.));
#10442=DIRECTION('center_axis',(0.,-1.,0.));
#10443=DIRECTION('ref_axis',(1.,0.,0.));
#10444=DIRECTION('',(1.,0.,0.));
#10445=DIRECTION('',(1.,0.,0.));
#10446=DIRECTION('',(0.,0.,1.));
#10447=DIRECTION('center_axis',(-1.,0.,0.));
#10448=DIRECTION('ref_axis',(0.,-1.,0.));
#10449=DIRECTION('',(0.,-1.,0.));
#10450=DIRECTION('',(0.,-1.,0.));
#10451=DIRECTION('center_axis',(0.,0.,1.));
#10452=DIRECTION('ref_axis',(1.,0.,0.));
#10453=DIRECTION('center_axis',(0.,0.,1.));
#10454=DIRECTION('ref_axis',(1.,0.,0.));
#10455=DIRECTION('axis',(0.,0.,1.));
#10456=DIRECTION('refdir',(1.,0.,0.));
#10457=DIRECTION('center_axis',(0.,0.,1.));
#10458=DIRECTION('ref_axis',(1.,0.,0.));
#10459=DIRECTION('center_axis',(0.,0.,1.));
#10460=DIRECTION('ref_axis',(1.,0.,0.));
#10461=DIRECTION('',(0.,0.,1.));
#10462=DIRECTION('center_axis',(0.,0.,1.));
#10463=DIRECTION('ref_axis',(1.,0.,0.));
#10464=DIRECTION('center_axis',(0.,0.,1.));
#10465=DIRECTION('ref_axis',(1.,0.,0.));
#10466=DIRECTION('center_axis',(0.,0.,1.));
#10467=DIRECTION('ref_axis',(1.,0.,0.));
#10468=DIRECTION('center_axis',(0.,0.,1.));
#10469=DIRECTION('ref_axis',(1.,0.,0.));
#10470=DIRECTION('',(0.,0.,1.));
#10471=DIRECTION('center_axis',(0.,0.,1.));
#10472=DIRECTION('ref_axis',(1.,0.,0.));
#10473=DIRECTION('center_axis',(0.,0.,1.));
#10474=DIRECTION('ref_axis',(1.,0.,0.));
#10475=DIRECTION('center_axis',(0.,1.,0.));
#10476=DIRECTION('ref_axis',(-1.,0.,0.));
#10477=DIRECTION('',(-1.,0.,0.));
#10478=DIRECTION('',(0.,0.,1.));
#10479=DIRECTION('',(-1.,0.,0.));
#10480=DIRECTION('',(0.,0.,1.));
#10481=DIRECTION('center_axis',(1.,0.,0.));
#10482=DIRECTION('ref_axis',(0.,1.,0.));
#10483=DIRECTION('',(0.,1.,0.));
#10484=DIRECTION('',(0.,1.,0.));
#10485=DIRECTION('',(0.,0.,1.));
#10486=DIRECTION('center_axis',(0.,-1.,0.));
#10487=DIRECTION('ref_axis',(1.,0.,0.));
#10488=DIRECTION('',(1.,0.,0.));
#10489=DIRECTION('',(1.,0.,0.));
#10490=DIRECTION('',(0.,0.,1.));
#10491=DIRECTION('center_axis',(-1.,0.,0.));
#10492=DIRECTION('ref_axis',(0.,-1.,0.));
#10493=DIRECTION('',(0.,-1.,0.));
#10494=DIRECTION('',(0.,-1.,0.));
#10495=DIRECTION('center_axis',(0.,0.,1.));
#10496=DIRECTION('ref_axis',(1.,0.,0.));
#10497=DIRECTION('center_axis',(0.,0.,1.));
#10498=DIRECTION('ref_axis',(1.,0.,0.));
#10499=DIRECTION('axis',(0.,0.,1.));
#10500=DIRECTION('refdir',(1.,0.,0.));
#10501=DIRECTION('center_axis',(0.,1.,0.));
#10502=DIRECTION('ref_axis',(1.,0.,0.));
#10503=DIRECTION('center_axis',(0.,1.,0.));
#10504=DIRECTION('ref_axis',(1.,0.,0.));
#10505=DIRECTION('',(0.,1.,0.));
#10506=DIRECTION('center_axis',(0.,-1.,0.));
#10507=DIRECTION('ref_axis',(1.,0.,0.));
#10508=DIRECTION('center_axis',(0.,1.,0.));
#10509=DIRECTION('ref_axis',(1.,0.,0.));
#10510=DIRECTION('center_axis',(0.,1.,0.));
#10511=DIRECTION('ref_axis',(1.,0.,0.));
#10512=DIRECTION('center_axis',(0.,1.,0.));
#10513=DIRECTION('ref_axis',(1.,0.,0.));
#10514=DIRECTION('center_axis',(0.,1.,0.));
#10515=DIRECTION('ref_axis',(1.,0.,0.));
#10516=DIRECTION('center_axis',(0.,1.,0.));
#10517=DIRECTION('ref_axis',(1.,0.,0.));
#10518=DIRECTION('center_axis',(0.,1.,0.));
#10519=DIRECTION('ref_axis',(1.,0.,0.));
#10520=DIRECTION('',(0.,-1.,0.));
#10521=DIRECTION('center_axis',(0.,1.,0.));
#10522=DIRECTION('ref_axis',(1.,0.,0.));
#10523=DIRECTION('center_axis',(0.,1.,0.));
#10524=DIRECTION('ref_axis',(1.,0.,0.));
#10525=DIRECTION('',(0.,-1.,0.));
#10526=DIRECTION('center_axis',(0.,1.,0.));
#10527=DIRECTION('ref_axis',(1.,0.,0.));
#10528=DIRECTION('center_axis',(0.,1.,0.));
#10529=DIRECTION('ref_axis',(1.,0.,0.));
#10530=DIRECTION('axis',(0.,0.,1.));
#10531=DIRECTION('refdir',(1.,0.,0.));
#10532=DIRECTION('center_axis',(0.,0.,-1.));
#10533=DIRECTION('ref_axis',(0.,1.,0.));
#10534=DIRECTION('',(0.,1.,0.));
#10535=DIRECTION('',(1.,0.,0.));
#10536=DIRECTION('',(0.,-1.,0.));
#10537=DIRECTION('',(1.,0.,0.));
#10538=DIRECTION('center_axis',(0.,1.,-8.88178419700125E-16));
#10539=DIRECTION('ref_axis',(0.,8.88178419700125E-16,1.));
#10540=DIRECTION('',(0.,8.88178419700125E-16,1.));
#10541=DIRECTION('',(1.,0.,0.));
#10542=DIRECTION('',(0.,-8.88178419700125E-16,-1.));
#10543=DIRECTION('center_axis',(0.,-7.40148683083439E-16,-1.));
#10544=DIRECTION('ref_axis',(0.,1.,-7.40148683083439E-16));
#10545=DIRECTION('',(0.,1.,-7.40148683083439E-16));
#10546=DIRECTION('',(1.,0.,0.));
#10547=DIRECTION('',(0.,-1.,7.40148683083439E-16));
#10548=DIRECTION('center_axis',(0.,-0.707106781186547,-0.707106781186548));
#10549=DIRECTION('ref_axis',(0.,0.707106781186548,-0.707106781186547));
#10550=DIRECTION('',(0.,0.707106781186548,-0.707106781186547));
#10551=DIRECTION('',(1.,0.,0.));
#10552=DIRECTION('',(0.,-0.707106781186548,0.707106781186547));
#10553=DIRECTION('center_axis',(0.,-1.,2.77555756156289E-16));
#10554=DIRECTION('ref_axis',(0.,-2.77555756156289E-16,-1.));
#10555=DIRECTION('',(0.,-2.77555756156289E-16,-1.));
#10556=DIRECTION('',(1.,0.,0.));
#10557=DIRECTION('',(0.,2.77555756156289E-16,1.));
#10558=DIRECTION('center_axis',(0.,-0.707106781186547,0.707106781186548));
#10559=DIRECTION('ref_axis',(0.,-0.707106781186548,-0.707106781186547));
#10560=DIRECTION('',(0.,-0.707106781186548,-0.707106781186547));
#10561=DIRECTION('',(1.,0.,0.));
#10562=DIRECTION('',(0.,0.707106781186548,0.707106781186547));
#10563=DIRECTION('center_axis',(0.,7.40148683083438E-16,1.));
#10564=DIRECTION('ref_axis',(0.,-1.,7.40148683083438E-16));
#10565=DIRECTION('',(0.,-1.,7.40148683083438E-16));
#10566=DIRECTION('',(1.,0.,0.));
#10567=DIRECTION('',(0.,1.,-7.40148683083438E-16));
#10568=DIRECTION('center_axis',(0.,1.,-4.44089209850063E-16));
#10569=DIRECTION('ref_axis',(0.,4.44089209850063E-16,1.));
#10570=DIRECTION('',(0.,4.44089209850063E-16,1.));
#10571=DIRECTION('',(1.,0.,0.));
#10572=DIRECTION('',(0.,-4.44089209850063E-16,-1.));
#10573=DIRECTION('center_axis',(0.,2.41352831440251E-16,1.));
#10574=DIRECTION('ref_axis',(0.,-1.,2.41352831440251E-16));
#10575=DIRECTION('',(0.,-1.,2.41352831440251E-16));
#10576=DIRECTION('',(-1.,0.,0.));
#10577=DIRECTION('',(0.,1.,-2.41352831440251E-16));
#10578=DIRECTION('center_axis',(0.,-1.,2.41352831440251E-16));
#10579=DIRECTION('ref_axis',(0.,-2.41352831440251E-16,-1.));
#10580=DIRECTION('',(0.,-2.41352831440251E-16,-1.));
#10581=DIRECTION('',(1.,0.,0.));
#10582=DIRECTION('',(0.,2.41352831440251E-16,1.));
#10583=DIRECTION('',(1.,0.,0.));
#10584=DIRECTION('center_axis',(0.,0.,-1.));
#10585=DIRECTION('ref_axis',(0.,1.,0.));
#10586=DIRECTION('',(0.,1.,0.));
#10587=DIRECTION('',(1.,0.,0.));
#10588=DIRECTION('',(0.,-1.,0.));
#10589=DIRECTION('center_axis',(0.,-1.,0.));
#10590=DIRECTION('ref_axis',(0.,0.,-1.));
#10591=DIRECTION('',(0.,0.,-1.));
#10592=DIRECTION('',(1.,0.,0.));
#10593=DIRECTION('',(0.,0.,1.));
#10594=DIRECTION('center_axis',(0.,-0.707106781186547,0.707106781186548));
#10595=DIRECTION('ref_axis',(0.,-0.707106781186548,-0.707106781186547));
#10596=DIRECTION('',(0.,-0.707106781186548,-0.707106781186547));
#10597=DIRECTION('',(1.,0.,0.));
#10598=DIRECTION('',(0.,0.707106781186548,0.707106781186547));
#10599=DIRECTION('center_axis',(0.,0.,1.));
#10600=DIRECTION('ref_axis',(0.,-1.,0.));
#10601=DIRECTION('',(0.,-1.,0.));
#10602=DIRECTION('',(1.,0.,0.));
#10603=DIRECTION('',(0.,1.,0.));
#10604=DIRECTION('center_axis',(0.,0.707106781186548,0.707106781186547));
#10605=DIRECTION('ref_axis',(0.,-0.707106781186547,0.707106781186548));
#10606=DIRECTION('',(0.,-0.707106781186547,0.707106781186548));
#10607=DIRECTION('',(1.,0.,0.));
#10608=DIRECTION('',(0.,0.707106781186547,-0.707106781186548));
#10609=DIRECTION('center_axis',(0.,1.,0.));
#10610=DIRECTION('ref_axis',(0.,0.,1.));
#10611=DIRECTION('',(0.,0.,1.));
#10612=DIRECTION('',(1.,0.,0.));
#10613=DIRECTION('',(0.,0.,-1.));
#10614=DIRECTION('center_axis',(0.,0.,-1.));
#10615=DIRECTION('ref_axis',(0.,1.,0.));
#10616=DIRECTION('',(0.,1.,0.));
#10617=DIRECTION('',(1.,0.,0.));
#10618=DIRECTION('',(0.,-1.,0.));
#10619=DIRECTION('center_axis',(0.,1.,-2.41352831440251E-16));
#10620=DIRECTION('ref_axis',(0.,2.41352831440251E-16,1.));
#10621=DIRECTION('',(0.,2.41352831440251E-16,1.));
#10622=DIRECTION('',(-1.,0.,0.));
#10623=DIRECTION('',(0.,-2.41352831440251E-16,-1.));
#10624=DIRECTION('center_axis',(0.,0.,1.));
#10625=DIRECTION('ref_axis',(0.,-1.,0.));
#10626=DIRECTION('',(0.,-1.,0.));
#10627=DIRECTION('',(1.,0.,0.));
#10628=DIRECTION('',(0.,1.,0.));
#10629=DIRECTION('',(1.,0.,0.));
#10630=DIRECTION('center_axis',(0.,-1.,0.));
#10631=DIRECTION('ref_axis',(0.,0.,-1.));
#10632=DIRECTION('',(0.,0.,-1.));
#10633=DIRECTION('',(1.,0.,0.));
#10634=DIRECTION('',(0.,0.,1.));
#10635=DIRECTION('center_axis',(0.,0.,1.));
#10636=DIRECTION('ref_axis',(0.,-1.,0.));
#10637=DIRECTION('',(0.,-1.,0.));
#10638=DIRECTION('',(1.,0.,0.));
#10639=DIRECTION('',(0.,1.,0.));
#10640=DIRECTION('center_axis',(0.,0.707106781186548,0.707106781186548));
#10641=DIRECTION('ref_axis',(0.,-0.707106781186548,0.707106781186548));
#10642=DIRECTION('',(0.,-0.707106781186548,0.707106781186548));
#10643=DIRECTION('',(1.,0.,0.));
#10644=DIRECTION('',(0.,0.707106781186548,-0.707106781186548));
#10645=DIRECTION('center_axis',(0.,1.,0.));
#10646=DIRECTION('ref_axis',(0.,0.,1.));
#10647=DIRECTION('',(0.,0.,1.));
#10648=DIRECTION('',(1.,0.,0.));
#10649=DIRECTION('',(0.,0.,-1.));
#10650=DIRECTION('center_axis',(0.,0.707106781186548,-0.707106781186547));
#10651=DIRECTION('ref_axis',(0.,0.707106781186547,0.707106781186548));
#10652=DIRECTION('',(0.,0.707106781186547,0.707106781186548));
#10653=DIRECTION('',(1.,0.,0.));
#10654=DIRECTION('',(0.,-0.707106781186547,-0.707106781186548));
#10655=DIRECTION('center_axis',(0.,-7.40148683083438E-16,-1.));
#10656=DIRECTION('ref_axis',(0.,1.,-7.40148683083438E-16));
#10657=DIRECTION('',(0.,1.,-7.40148683083438E-16));
#10658=DIRECTION('',(1.,0.,0.));
#10659=DIRECTION('',(0.,-1.,7.40148683083438E-16));
#10660=DIRECTION('center_axis',(0.,-1.,0.));
#10661=DIRECTION('ref_axis',(0.,0.,-1.));
#10662=DIRECTION('',(0.,0.,-1.));
#10663=DIRECTION('',(1.,0.,0.));
#10664=DIRECTION('',(0.,0.,1.));
#10665=DIRECTION('center_axis',(0.,0.,-1.));
#10666=DIRECTION('ref_axis',(0.,1.,0.));
#10667=DIRECTION('',(0.,1.,0.));
#10668=DIRECTION('',(-1.,0.,0.));
#10669=DIRECTION('',(0.,-1.,0.));
#10670=DIRECTION('center_axis',(0.,1.,0.));
#10671=DIRECTION('ref_axis',(0.,0.,1.));
#10672=DIRECTION('',(0.,0.,1.));
#10673=DIRECTION('',(1.,0.,0.));
#10674=DIRECTION('',(0.,0.,-1.));
#10675=DIRECTION('',(1.,0.,0.));
#10676=DIRECTION('center_axis',(0.,0.,1.));
#10677=DIRECTION('ref_axis',(0.,-1.,0.));
#10678=DIRECTION('',(0.,-1.,0.));
#10679=DIRECTION('',(1.,0.,0.));
#10680=DIRECTION('',(0.,1.,0.));
#10681=DIRECTION('center_axis',(0.,1.,0.));
#10682=DIRECTION('ref_axis',(0.,0.,1.));
#10683=DIRECTION('',(0.,0.,1.));
#10684=DIRECTION('',(1.,0.,0.));
#10685=DIRECTION('',(0.,0.,-1.));
#10686=DIRECTION('center_axis',(0.,0.707106781186547,-0.707106781186548));
#10687=DIRECTION('ref_axis',(0.,0.707106781186548,0.707106781186547));
#10688=DIRECTION('',(0.,0.707106781186548,0.707106781186547));
#10689=DIRECTION('',(1.,0.,0.));
#10690=DIRECTION('',(0.,-0.707106781186548,-0.707106781186547));
#10691=DIRECTION('center_axis',(0.,0.,-1.));
#10692=DIRECTION('ref_axis',(0.,1.,0.));
#10693=DIRECTION('',(0.,1.,0.));
#10694=DIRECTION('',(1.,0.,0.));
#10695=DIRECTION('',(0.,-1.,0.));
#10696=DIRECTION('center_axis',(0.,-0.707106781186547,-0.707106781186548));
#10697=DIRECTION('ref_axis',(0.,0.707106781186548,-0.707106781186547));
#10698=DIRECTION('',(0.,0.707106781186548,-0.707106781186547));
#10699=DIRECTION('',(1.,0.,0.));
#10700=DIRECTION('',(0.,-0.707106781186548,0.707106781186547));
#10701=DIRECTION('center_axis',(0.,-1.,0.));
#10702=DIRECTION('ref_axis',(0.,0.,-1.));
#10703=DIRECTION('',(0.,0.,-1.));
#10704=DIRECTION('',(1.,0.,0.));
#10705=DIRECTION('',(0.,0.,1.));
#10706=DIRECTION('center_axis',(0.,0.,1.));
#10707=DIRECTION('ref_axis',(0.,-1.,0.));
#10708=DIRECTION('',(0.,-1.,0.));
#10709=DIRECTION('',(1.,0.,0.));
#10710=DIRECTION('',(0.,1.,0.));
#10711=DIRECTION('center_axis',(0.,-1.,0.));
#10712=DIRECTION('ref_axis',(0.,0.,-1.));
#10713=DIRECTION('',(0.,0.,-1.));
#10714=DIRECTION('',(-1.,0.,0.));
#10715=DIRECTION('',(0.,0.,1.));
#10716=DIRECTION('center_axis',(1.,0.,0.));
#10717=DIRECTION('ref_axis',(0.,0.,-1.));
#10718=DIRECTION('center_axis',(1.,0.,0.));
#10719=DIRECTION('ref_axis',(0.,0.,-1.));
#10720=DIRECTION('',(1.,0.,0.));
#10721=DIRECTION('center_axis',(-1.,0.,0.));
#10722=DIRECTION('ref_axis',(0.,0.,-1.));
#10723=DIRECTION('center_axis',(0.,1.,0.));
#10724=DIRECTION('ref_axis',(0.,0.,1.));
#10725=DIRECTION('',(0.,0.,1.));
#10726=DIRECTION('',(1.,0.,0.));
#10727=DIRECTION('',(0.,0.,1.));
#10728=DIRECTION('center_axis',(0.,1.,0.));
#10729=DIRECTION('ref_axis',(0.,0.,1.));
#10730=DIRECTION('',(0.,0.,1.));
#10731=DIRECTION('',(1.,0.,0.));
#10732=DIRECTION('',(0.,0.,1.));
#10733=DIRECTION('center_axis',(0.,0.,-1.));
#10734=DIRECTION('ref_axis',(0.,1.,0.));
#10735=DIRECTION('',(0.,1.,0.));
#10736=DIRECTION('',(0.,1.,0.));
#10737=DIRECTION('center_axis',(0.,0.,-1.));
#10738=DIRECTION('ref_axis',(0.,1.,0.));
#10739=DIRECTION('',(0.,1.,0.));
#10740=DIRECTION('',(1.,0.,0.));
#10741=DIRECTION('',(0.,1.,0.));
#10742=DIRECTION('center_axis',(0.,-1.,0.));
#10743=DIRECTION('ref_axis',(0.,0.,-1.));
#10744=DIRECTION('',(0.,0.,-1.));
#10745=DIRECTION('',(0.,0.,-1.));
#10746=DIRECTION('center_axis',(0.,-1.,0.));
#10747=DIRECTION('ref_axis',(0.,0.,-1.));
#10748=DIRECTION('',(0.,0.,-1.));
#10749=DIRECTION('',(1.,0.,0.));
#10750=DIRECTION('',(0.,0.,-1.));
#10751=DIRECTION('center_axis',(0.,0.,1.));
#10752=DIRECTION('ref_axis',(0.,-1.,0.));
#10753=DIRECTION('',(0.,-1.,0.));
#10754=DIRECTION('',(0.,-1.,0.));
#10755=DIRECTION('center_axis',(0.,0.,1.));
#10756=DIRECTION('ref_axis',(0.,-1.,0.));
#10757=DIRECTION('',(0.,-1.,0.));
#10758=DIRECTION('',(0.,-1.,0.));
#10759=DIRECTION('center_axis',(1.,0.,0.));
#10760=DIRECTION('ref_axis',(0.,0.,-1.));
#10761=DIRECTION('center_axis',(1.,0.,0.));
#10762=DIRECTION('ref_axis',(0.,0.,-1.));
#10763=DIRECTION('axis',(0.,0.,1.));
#10764=DIRECTION('refdir',(1.,0.,0.));
#10765=DIRECTION('center_axis',(0.,0.,1.));
#10766=DIRECTION('ref_axis',(1.,0.,0.));
#10767=DIRECTION('',(1.,0.,0.));
#10768=DIRECTION('',(0.,-1.,0.));
#10769=DIRECTION('',(-1.,0.,0.));
#10770=DIRECTION('',(0.,1.,0.));
#10771=DIRECTION('center_axis',(0.,1.,0.));
#10772=DIRECTION('ref_axis',(-1.,0.,0.));
#10773=DIRECTION('',(0.,0.,1.));
#10774=DIRECTION('',(-1.,0.,0.));
#10775=DIRECTION('',(0.,0.,1.));
#10776=DIRECTION('center_axis',(0.,0.,1.));
#10777=DIRECTION('ref_axis',(1.,0.,0.));
#10778=DIRECTION('',(0.,-1.,0.));
#10779=DIRECTION('',(1.,0.,0.));
#10780=DIRECTION('',(0.,1.,0.));
#10781=DIRECTION('center_axis',(0.,0.,-1.));
#10782=DIRECTION('ref_axis',(1.,0.,0.));
#10783=DIRECTION('center_axis',(-1.,0.,0.));
#10784=DIRECTION('ref_axis',(0.,-1.,0.));
#10785=DIRECTION('',(0.,0.,1.));
#10786=DIRECTION('',(0.,0.707106781186548,0.707106781186548));
#10787=DIRECTION('',(0.,-1.,0.));
#10788=DIRECTION('',(0.,0.707106781186548,-0.707106781186548));
#10789=DIRECTION('',(0.,0.,1.));
#10790=DIRECTION('',(0.,-1.,0.));
#10791=DIRECTION('',(0.,0.,1.));
#10792=DIRECTION('center_axis',(0.,-1.,0.));
#10793=DIRECTION('ref_axis',(1.,0.,0.));
#10794=DIRECTION('',(1.,0.,0.));
#10795=DIRECTION('',(0.,0.,1.));
#10796=DIRECTION('center_axis',(0.,0.,1.));
#10797=DIRECTION('ref_axis',(1.,0.,0.));
#10798=DIRECTION('',(-1.,0.,0.));
#10799=DIRECTION('',(0.,1.,0.));
#10800=DIRECTION('center_axis',(1.,0.,0.));
#10801=DIRECTION('ref_axis',(0.,1.,0.));
#10802=DIRECTION('',(0.,0.,1.));
#10803=DIRECTION('',(0.,-0.707106781186548,0.707106781186548));
#10804=DIRECTION('',(0.,1.,0.));
#10805=DIRECTION('',(0.,-0.707106781186548,-0.707106781186548));
#10806=DIRECTION('',(0.,0.,1.));
#10807=DIRECTION('center_axis',(0.,-1.,0.));
#10808=DIRECTION('ref_axis',(1.,0.,0.));
#10809=DIRECTION('',(-1.,0.,0.));
#10810=DIRECTION('center_axis',(0.,-0.707106781186548,-0.707106781186548));
#10811=DIRECTION('ref_axis',(-1.,0.,0.));
#10812=DIRECTION('',(1.,0.,0.));
#10813=DIRECTION('center_axis',(0.,0.707106781186548,0.707106781186548));
#10814=DIRECTION('ref_axis',(0.,0.707106781186547,-0.707106781186547));
#10815=DIRECTION('',(1.,0.,0.));
#10816=DIRECTION('center_axis',(0.,0.,1.));
#10817=DIRECTION('ref_axis',(1.,0.,0.));
#10818=DIRECTION('center_axis',(0.,0.,-1.));
#10819=DIRECTION('ref_axis',(1.,0.,0.));
#10820=DIRECTION('',(0.,0.,1.));
#10821=DIRECTION('center_axis',(0.,0.,-1.));
#10822=DIRECTION('ref_axis',(1.,0.,0.));
#10823=DIRECTION('center_axis',(0.,-0.707106781186548,0.707106781186548));
#10824=DIRECTION('ref_axis',(0.,0.707106781186547,0.707106781186547));
#10825=DIRECTION('center_axis',(0.,0.,-1.));
#10826=DIRECTION('ref_axis',(1.,0.,0.));
#10827=DIRECTION('center_axis',(0.,0.,1.));
#10828=DIRECTION('ref_axis',(1.,0.,0.));
#10829=DIRECTION('',(-1.,0.,0.));
#10830=DIRECTION('center_axis',(0.,0.,1.));
#10831=DIRECTION('ref_axis',(1.,0.,0.));
#10832=DIRECTION('',(-1.,0.,0.));
#10833=DIRECTION('center_axis',(0.,0.707106781186548,-0.707106781186548));
#10834=DIRECTION('ref_axis',(-1.,0.,0.));
#10835=DIRECTION('',(1.,0.,0.));
#10836=DIRECTION('center_axis',(0.,1.,0.));
#10837=DIRECTION('ref_axis',(-1.,0.,0.));
#10838=DIRECTION('axis',(0.,0.,1.));
#10839=DIRECTION('refdir',(1.,0.,0.));
#10840=DIRECTION('center_axis',(0.,1.,0.));
#10841=DIRECTION('ref_axis',(1.,0.,0.));
#10842=DIRECTION('center_axis',(0.,1.,0.));
#10843=DIRECTION('ref_axis',(1.,0.,0.));
#10844=DIRECTION('',(0.707106781186548,-0.707106781186547,-8.65956056235494E-17));
#10845=DIRECTION('center_axis',(0.,-1.,0.));
#10846=DIRECTION('ref_axis',(1.,0.,0.));
#10847=DIRECTION('center_axis',(0.,1.,0.));
#10848=DIRECTION('ref_axis',(1.,0.,0.));
#10849=DIRECTION('',(0.,-1.,0.));
#10850=DIRECTION('center_axis',(0.,-1.,0.));
#10851=DIRECTION('ref_axis',(1.,0.,0.));
#10852=DIRECTION('center_axis',(0.,1.,0.));
#10853=DIRECTION('ref_axis',(1.,0.,0.));
#10854=DIRECTION('center_axis',(0.,1.,0.));
#10855=DIRECTION('ref_axis',(1.,0.,0.));
#10856=DIRECTION('center_axis',(0.,1.,0.));
#10857=DIRECTION('ref_axis',(1.,0.,0.));
#10858=DIRECTION('',(0.,-1.,0.));
#10859=DIRECTION('center_axis',(0.,1.,0.));
#10860=DIRECTION('ref_axis',(1.,0.,0.));
#10861=DIRECTION('center_axis',(0.,1.,0.));
#10862=DIRECTION('ref_axis',(1.,0.,0.));
#10863=DIRECTION('axis',(0.,0.,1.));
#10864=DIRECTION('refdir',(1.,0.,0.));
#10865=DIRECTION('center_axis',(0.866025403784439,0.,-0.5));
#10866=DIRECTION('ref_axis',(0.5,0.,0.866025403784439));
#10867=DIRECTION('',(-0.5,0.,-0.866025403784439));
#10868=DIRECTION('',(0.,-1.,0.));
#10869=DIRECTION('',(0.5,0.,0.866025403784439));
#10870=DIRECTION('',(0.,-1.,0.));
#10871=DIRECTION('center_axis',(1.20185167898973E-16,0.,-1.));
#10872=DIRECTION('ref_axis',(1.,0.,1.20185167898973E-16));
#10873=DIRECTION('',(-1.,0.,-1.20185167898973E-16));
#10874=DIRECTION('',(0.,-1.,0.));
#10875=DIRECTION('',(1.,0.,1.20185167898973E-16));
#10876=DIRECTION('center_axis',(-0.866025403784439,0.,-0.5));
#10877=DIRECTION('ref_axis',(0.5,0.,-0.866025403784439));
#10878=DIRECTION('',(-0.5,0.,0.866025403784439));
#10879=DIRECTION('',(0.,-1.,0.));
#10880=DIRECTION('',(0.5,0.,-0.866025403784439));
#10881=DIRECTION('center_axis',(-0.866025403784439,0.,0.5));
#10882=DIRECTION('ref_axis',(-0.5,0.,-0.866025403784439));
#10883=DIRECTION('',(0.5,0.,0.866025403784439));
#10884=DIRECTION('',(0.,-1.,0.));
#10885=DIRECTION('',(-0.5,0.,-0.866025403784439));
#10886=DIRECTION('center_axis',(-2.40370335797945E-16,0.,1.));
#10887=DIRECTION('ref_axis',(-1.,0.,-2.40370335797945E-16));
#10888=DIRECTION('',(1.,0.,2.40370335797945E-16));
#10889=DIRECTION('',(0.,-1.,0.));
#10890=DIRECTION('',(-1.,0.,-2.40370335797945E-16));
#10891=DIRECTION('center_axis',(0.866025403784439,0.,0.5));
#10892=DIRECTION('ref_axis',(-0.5,0.,0.866025403784439));
#10893=DIRECTION('',(0.5,0.,-0.866025403784439));
#10894=DIRECTION('',(-0.5,0.,0.866025403784439));
#10895=DIRECTION('center_axis',(0.,1.,0.));
#10896=DIRECTION('ref_axis',(1.,0.,0.));
#10897=DIRECTION('center_axis',(0.,-1.,0.));
#10898=DIRECTION('ref_axis',(0.,0.,-1.));
#10899=DIRECTION('center_axis',(0.,1.,0.));
#10900=DIRECTION('ref_axis',(1.,0.,0.));
#10901=DIRECTION('center_axis',(0.,1.,0.));
#10902=DIRECTION('ref_axis',(1.,0.,0.));
#10903=DIRECTION('center_axis',(0.,1.,0.));
#10904=DIRECTION('ref_axis',(0.,0.,1.));
#10905=DIRECTION('center_axis',(0.,-1.,0.));
#10906=DIRECTION('ref_axis',(1.,0.,0.));
#10907=DIRECTION('center_axis',(0.,-1.,0.));
#10908=DIRECTION('ref_axis',(1.,0.,0.));
#10909=DIRECTION('center_axis',(0.,-1.,0.));
#10910=DIRECTION('ref_axis',(1.,0.,0.));
#10911=DIRECTION('',(0.707106781186548,0.707106781186547,8.65956056235493E-17));
#10912=DIRECTION('center_axis',(0.,-1.,0.));
#10913=DIRECTION('ref_axis',(1.,0.,0.));
#10914=DIRECTION('center_axis',(0.,-1.,0.));
#10915=DIRECTION('ref_axis',(1.,0.,0.));
#10916=DIRECTION('',(0.,1.,0.));
#10917=DIRECTION('center_axis',(0.,1.,0.));
#10918=DIRECTION('ref_axis',(1.,0.,0.));
#10919=DIRECTION('center_axis',(0.,-1.,0.));
#10920=DIRECTION('ref_axis',(1.,0.,0.));
#10921=DIRECTION('',(-0.707106781186547,0.707106781186548,-8.65956056235493E-17));
#10922=DIRECTION('center_axis',(0.,-1.,0.));
#10923=DIRECTION('ref_axis',(0.,0.,-1.));
#10924=DIRECTION('center_axis',(0.,-1.,0.));
#10925=DIRECTION('ref_axis',(1.,0.,0.));
#10926=DIRECTION('center_axis',(0.,1.,0.));
#10927=DIRECTION('ref_axis',(1.,0.,0.));
#10928=DIRECTION('center_axis',(0.,1.,0.));
#10929=DIRECTION('ref_axis',(1.,0.,0.));
#10930=DIRECTION('',(-0.447213595499958,0.894427190999916,-5.47678698264203E-17));
#10931=DIRECTION('center_axis',(0.,-1.,0.));
#10932=DIRECTION('ref_axis',(1.,0.,0.));
#10933=DIRECTION('',(0.,1.,0.));
#10934=DIRECTION('axis',(0.,0.,1.));
#10935=DIRECTION('refdir',(1.,0.,0.));
#10936=DIRECTION('axis',(0.,0.,1.));
#10937=DIRECTION('refdir',(1.,0.,0.));
#10938=DIRECTION('center_axis',(0.,-1.,0.));
#10939=DIRECTION('ref_axis',(0.,0.,-1.));
#10940=DIRECTION('center_axis',(0.,-1.,0.));
#10941=DIRECTION('ref_axis',(1.,0.,0.));
#10942=DIRECTION('center_axis',(0.,-1.,0.));
#10943=DIRECTION('ref_axis',(1.,0.,0.));
#10944=DIRECTION('center_axis',(1.,0.,1.22464679914735E-16));
#10945=DIRECTION('ref_axis',(-1.22464679914735E-16,0.,1.));
#10946=DIRECTION('center_axis',(0.,1.,0.));
#10947=DIRECTION('ref_axis',(1.,0.,0.));
#10948=DIRECTION('center_axis',(0.,1.,0.));
#10949=DIRECTION('ref_axis',(1.,0.,0.));
#10950=DIRECTION('center_axis',(0.,-1.,0.));
#10951=DIRECTION('ref_axis',(1.,0.,0.));
#10952=DIRECTION('',(0.,1.,0.));
#10953=DIRECTION('center_axis',(0.,-1.,0.));
#10954=DIRECTION('ref_axis',(1.,0.,0.));
#10955=DIRECTION('center_axis',(0.,-1.,0.));
#10956=DIRECTION('ref_axis',(1.,0.,0.));
#10957=DIRECTION('center_axis',(0.,-1.,0.));
#10958=DIRECTION('ref_axis',(1.,0.,0.));
#10959=DIRECTION('',(0.,1.,0.));
#10960=DIRECTION('center_axis',(0.,-1.,0.));
#10961=DIRECTION('ref_axis',(1.,0.,0.));
#10962=DIRECTION('center_axis',(0.,1.,0.));
#10963=DIRECTION('ref_axis',(1.,0.,0.));
#10964=DIRECTION('',(-0.707106781186547,0.707106781186548,-8.65956056235493E-17));
#10965=DIRECTION('center_axis',(0.,-1.,0.));
#10966=DIRECTION('ref_axis',(1.,0.,0.));
#10967=DIRECTION('center_axis',(0.,1.,0.));
#10968=DIRECTION('ref_axis',(0.,0.,1.));
#10969=DIRECTION('center_axis',(0.,-1.,0.));
#10970=DIRECTION('ref_axis',(1.,0.,0.));
#10971=DIRECTION('center_axis',(0.,-1.,0.));
#10972=DIRECTION('ref_axis',(1.,0.,0.));
#10973=DIRECTION('',(0.,1.,0.));
#10974=DIRECTION('center_axis',(0.,-1.,0.));
#10975=DIRECTION('ref_axis',(0.,0.,-1.));
#10976=DIRECTION('center_axis',(0.,-1.,0.));
#10977=DIRECTION('ref_axis',(1.,0.,0.));
#10978=DIRECTION('center_axis',(0.,-1.,0.));
#10979=DIRECTION('ref_axis',(1.,0.,0.));
#10980=DIRECTION('',(0.707106781186547,0.707106781186548,8.65956056235493E-17));
#10981=DIRECTION('axis',(0.,0.,1.));
#10982=DIRECTION('refdir',(1.,0.,0.));
#10983=DIRECTION('center_axis',(0.,-1.,0.));
#10984=DIRECTION('ref_axis',(0.,0.,-1.));
#10985=DIRECTION('center_axis',(0.,-1.,0.));
#10986=DIRECTION('ref_axis',(1.,0.,0.));
#10987=DIRECTION('center_axis',(0.,-1.,0.));
#10988=DIRECTION('ref_axis',(1.,0.,0.));
#10989=DIRECTION('center_axis',(1.,0.,1.22464679914735E-16));
#10990=DIRECTION('ref_axis',(-1.22464679914735E-16,0.,1.));
#10991=DIRECTION('center_axis',(0.,1.,0.));
#10992=DIRECTION('ref_axis',(1.,0.,0.));
#10993=DIRECTION('center_axis',(0.,1.,0.));
#10994=DIRECTION('ref_axis',(1.,0.,0.));
#10995=DIRECTION('center_axis',(0.,-1.,0.));
#10996=DIRECTION('ref_axis',(1.,0.,0.));
#10997=DIRECTION('center_axis',(0.,-1.,0.));
#10998=DIRECTION('ref_axis',(1.,0.,0.));
#10999=DIRECTION('',(0.,1.,0.));
#11000=DIRECTION('center_axis',(0.,1.,0.));
#11001=DIRECTION('ref_axis',(0.,0.,1.));
#11002=DIRECTION('center_axis',(0.,-1.,0.));
#11003=DIRECTION('ref_axis',(1.,0.,0.));
#11004=DIRECTION('center_axis',(0.,-1.,0.));
#11005=DIRECTION('ref_axis',(1.,0.,0.));
#11006=DIRECTION('center_axis',(0.,-1.,0.));
#11007=DIRECTION('ref_axis',(1.,0.,0.));
#11008=DIRECTION('center_axis',(0.,-1.,0.));
#11009=DIRECTION('ref_axis',(1.,0.,0.));
#11010=DIRECTION('',(0.707106781186548,0.707106781186547,8.65956056235494E-17));
#11011=DIRECTION('center_axis',(0.,-1.,0.));
#11012=DIRECTION('ref_axis',(1.,0.,0.));
#11013=DIRECTION('center_axis',(0.,-1.,0.));
#11014=DIRECTION('ref_axis',(1.,0.,0.));
#11015=DIRECTION('',(0.,1.,0.));
#11016=DIRECTION('center_axis',(0.,1.,0.));
#11017=DIRECTION('ref_axis',(1.,0.,0.));
#11018=DIRECTION('center_axis',(0.,-1.,0.));
#11019=DIRECTION('ref_axis',(1.,0.,0.));
#11020=DIRECTION('',(-0.707106781186548,0.707106781186547,-8.65956056235494E-17));
#11021=DIRECTION('center_axis',(0.,-1.,0.));
#11022=DIRECTION('ref_axis',(0.,0.,-1.));
#11023=DIRECTION('center_axis',(0.,-1.,0.));
#11024=DIRECTION('ref_axis',(1.,0.,0.));
#11025=DIRECTION('',(0.,1.,0.));
#11026=DIRECTION('axis',(0.,0.,1.));
#11027=DIRECTION('refdir',(1.,0.,0.));
#11028=DIRECTION('center_axis',(0.,0.,1.));
#11029=DIRECTION('ref_axis',(1.,0.,0.));
#11030=DIRECTION('center_axis',(1.22464679914735E-16,-1.,0.));
#11031=DIRECTION('ref_axis',(-1.,-1.22464679914735E-16,0.));
#11032=DIRECTION('center_axis',(0.707106781186548,0.,0.707106781186548));
#11033=DIRECTION('ref_axis',(0.707106781186548,0.,-0.707106781186548));
#11034=DIRECTION('center_axis',(8.65956056235494E-17,-1.,-8.65956056235493E-17));
#11035=DIRECTION('ref_axis',(-0.707106781186547,-1.22464679914735E-16,0.707106781186547));
#11036=DIRECTION('center_axis',(1.,0.,0.));
#11037=DIRECTION('ref_axis',(6.12323399573676E-17,0.,-1.));
#11038=DIRECTION('center_axis',(7.49879891330929E-33,-1.,-1.22464679914735E-16));
#11039=DIRECTION('ref_axis',(-6.12323399573676E-17,-1.22464679914735E-16,
1.));
#11040=DIRECTION('center_axis',(0.707106781186548,0.,-0.707106781186548));
#11041=DIRECTION('ref_axis',(-0.707106781186548,0.,-0.707106781186548));
#11042=DIRECTION('center_axis',(-8.65956056235493E-17,-1.,-8.65956056235494E-17));
#11043=DIRECTION('ref_axis',(0.707106781186547,-1.22464679914735E-16,0.707106781186547));
#11044=DIRECTION('center_axis',(0.,0.,-1.));
#11045=DIRECTION('ref_axis',(-1.,0.,-1.22464679914735E-16));
#11046=DIRECTION('center_axis',(-1.22464679914735E-16,-1.,-1.49975978266186E-32));
#11047=DIRECTION('ref_axis',(1.,-1.22464679914735E-16,1.22464679914735E-16));
#11048=DIRECTION('center_axis',(-0.707106781186547,0.,-0.707106781186548));
#11049=DIRECTION('ref_axis',(-0.707106781186548,0.,0.707106781186547));
#11050=DIRECTION('center_axis',(-8.65956056235493E-17,-1.,8.65956056235493E-17));
#11051=DIRECTION('ref_axis',(0.707106781186548,-1.22464679914735E-16,-0.707106781186547));
#11052=DIRECTION('center_axis',(-1.,0.,0.));
#11053=DIRECTION('ref_axis',(-1.83697019872103E-16,0.,1.));
#11054=DIRECTION('center_axis',(-2.24963967399279E-32,-1.,1.22464679914735E-16));
#11055=DIRECTION('ref_axis',(1.83697019872103E-16,-1.22464679914735E-16,
-1.));
#11056=DIRECTION('center_axis',(-0.707106781186548,0.,0.707106781186548));
#11057=DIRECTION('ref_axis',(0.707106781186547,0.,0.707106781186548));
#11058=DIRECTION('center_axis',(8.65956056235493E-17,-1.,8.65956056235493E-17));
#11059=DIRECTION('ref_axis',(-0.707106781186547,-1.22464679914735E-16,-0.707106781186548));
#11060=DIRECTION('axis',(0.,0.,1.));
#11061=DIRECTION('refdir',(1.,0.,0.));
#11062=DIRECTION('center_axis',(0.,0.,1.));
#11063=DIRECTION('ref_axis',(1.,0.,0.));
#11064=DIRECTION('center_axis',(0.,-1.,0.));
#11065=DIRECTION('ref_axis',(0.,0.,-1.));
#11066=DIRECTION('center_axis',(0.,-1.,0.));
#11067=DIRECTION('ref_axis',(0.,0.,-1.));
#11068=DIRECTION('center_axis',(0.,1.,0.));
#11069=DIRECTION('ref_axis',(1.,0.,0.));
#11070=DIRECTION('center_axis',(0.,1.,0.));
#11071=DIRECTION('ref_axis',(1.,0.,0.));
#11072=DIRECTION('center_axis',(0.,1.,0.));
#11073=DIRECTION('ref_axis',(1.,0.,0.));
#11074=DIRECTION('center_axis',(0.,1.,0.));
#11075=DIRECTION('ref_axis',(1.,0.,0.));
#11076=DIRECTION('',(0.,-1.,0.));
#11077=DIRECTION('center_axis',(0.,-1.,0.));
#11078=DIRECTION('ref_axis',(1.,0.,0.));
#11079=DIRECTION('center_axis',(0.,1.,0.));
#11080=DIRECTION('ref_axis',(1.,0.,0.));
#11081=DIRECTION('center_axis',(0.,1.,0.));
#11082=DIRECTION('ref_axis',(1.,0.,0.));
#11083=DIRECTION('center_axis',(0.,1.,0.));
#11084=DIRECTION('ref_axis',(1.,0.,0.));
#11085=DIRECTION('center_axis',(0.,1.,0.));
#11086=DIRECTION('ref_axis',(1.,0.,0.));
#11087=DIRECTION('center_axis',(0.,1.,0.));
#11088=DIRECTION('ref_axis',(1.,0.,0.));
#11089=DIRECTION('center_axis',(0.,1.,0.));
#11090=DIRECTION('ref_axis',(1.,0.,0.));
#11091=DIRECTION('center_axis',(0.,-1.,0.));
#11092=DIRECTION('ref_axis',(1.,0.,0.));
#11093=DIRECTION('center_axis',(0.,-1.,0.));
#11094=DIRECTION('ref_axis',(0.,0.,-1.));
#11095=DIRECTION('center_axis',(6.12323399573677E-17,0.,1.));
#11096=DIRECTION('ref_axis',(1.,0.,0.));
#11097=DIRECTION('center_axis',(0.,-1.,0.));
#11098=DIRECTION('ref_axis',(0.,0.,-1.));
#11099=DIRECTION('center_axis',(0.,1.,0.));
#11100=DIRECTION('ref_axis',(1.,0.,0.));
#11101=DIRECTION('center_axis',(0.,-1.,0.));
#11102=DIRECTION('ref_axis',(1.,0.,0.));
#11103=DIRECTION('center_axis',(0.,-1.,0.));
#11104=DIRECTION('ref_axis',(0.,0.,-1.));
#11105=DIRECTION('center_axis',(0.,0.,1.));
#11106=DIRECTION('ref_axis',(1.,0.,0.));
#11107=DIRECTION('center_axis',(0.,-1.,0.));
#11108=DIRECTION('ref_axis',(0.,0.,-1.));
#11109=DIRECTION('center_axis',(0.,1.,0.));
#11110=DIRECTION('ref_axis',(1.,0.,0.));
#11111=DIRECTION('center_axis',(0.,-1.,0.));
#11112=DIRECTION('ref_axis',(1.,0.,0.));
#11113=DIRECTION('center_axis',(0.,-1.,0.));
#11114=DIRECTION('ref_axis',(0.,0.,-1.));
#11115=DIRECTION('center_axis',(0.,0.,1.));
#11116=DIRECTION('ref_axis',(1.,0.,0.));
#11117=DIRECTION('center_axis',(0.,-1.,0.));
#11118=DIRECTION('ref_axis',(0.,0.,-1.));
#11119=DIRECTION('center_axis',(0.,1.,0.));
#11120=DIRECTION('ref_axis',(1.,0.,0.));
#11121=DIRECTION('center_axis',(0.,-1.,0.));
#11122=DIRECTION('ref_axis',(1.,0.,0.));
#11123=DIRECTION('center_axis',(0.,-1.,0.));
#11124=DIRECTION('ref_axis',(0.,0.,-1.));
#11125=DIRECTION('center_axis',(0.,0.,1.));
#11126=DIRECTION('ref_axis',(1.,0.,0.));
#11127=DIRECTION('center_axis',(0.,-1.,0.));
#11128=DIRECTION('ref_axis',(0.,0.,-1.));
#11129=DIRECTION('center_axis',(0.,1.,0.));
#11130=DIRECTION('ref_axis',(1.,0.,0.));
#11131=DIRECTION('center_axis',(0.,-1.,0.));
#11132=DIRECTION('ref_axis',(1.,0.,0.));
#11133=DIRECTION('center_axis',(0.,-1.,0.));
#11134=DIRECTION('ref_axis',(0.,0.,-1.));
#11135=DIRECTION('center_axis',(6.12323399573676E-17,0.,1.));
#11136=DIRECTION('ref_axis',(1.,0.,0.));
#11137=DIRECTION('center_axis',(0.,-1.,0.));
#11138=DIRECTION('ref_axis',(0.,0.,-1.));
#11139=DIRECTION('center_axis',(0.,1.,0.));
#11140=DIRECTION('ref_axis',(1.,0.,0.));
#11141=DIRECTION('center_axis',(0.,-1.,0.));
#11142=DIRECTION('ref_axis',(1.,0.,0.));
#11143=DIRECTION('center_axis',(0.,-1.,0.));
#11144=DIRECTION('ref_axis',(0.,0.,-1.));
#11145=DIRECTION('center_axis',(0.,0.,1.));
#11146=DIRECTION('ref_axis',(1.,0.,0.));
#11147=DIRECTION('center_axis',(0.,-1.,0.));
#11148=DIRECTION('ref_axis',(0.,0.,-1.));
#11149=DIRECTION('center_axis',(0.,1.,0.));
#11150=DIRECTION('ref_axis',(1.,0.,0.));
#11151=DIRECTION('center_axis',(0.,1.,0.));
#11152=DIRECTION('ref_axis',(1.,0.,0.));
#11153=DIRECTION('',(0.,1.,0.));
#11154=DIRECTION('center_axis',(0.,-1.,0.));
#11155=DIRECTION('ref_axis',(1.,0.,0.));
#11156=DIRECTION('center_axis',(0.,-1.,0.));
#11157=DIRECTION('ref_axis',(1.,0.,0.));
#11158=DIRECTION('center_axis',(0.,1.,0.));
#11159=DIRECTION('ref_axis',(1.,0.,0.));
#11160=DIRECTION('center_axis',(0.,-1.,0.));
#11161=DIRECTION('ref_axis',(0.,0.,-1.));
#11162=DIRECTION('center_axis',(0.,0.,1.));
#11163=DIRECTION('ref_axis',(1.,0.,0.));
#11164=DIRECTION('center_axis',(0.,-1.,0.));
#11165=DIRECTION('ref_axis',(0.,0.,-1.));
#11166=DIRECTION('center_axis',(0.,-1.,0.));
#11167=DIRECTION('ref_axis',(-1.,0.,0.));
#11168=DIRECTION('center_axis',(0.,1.,0.));
#11169=DIRECTION('ref_axis',(1.,0.,0.));
#11170=DIRECTION('axis',(0.,0.,1.));
#11171=DIRECTION('refdir',(1.,0.,0.));
#11172=DIRECTION('center_axis',(0.,1.,0.));
#11173=DIRECTION('ref_axis',(0.,0.,1.));
#11174=DIRECTION('center_axis',(0.,-1.,0.));
#11175=DIRECTION('ref_axis',(1.,0.,0.));
#11176=DIRECTION('center_axis',(0.,-1.,0.));
#11177=DIRECTION('ref_axis',(1.,0.,0.));
#11178=DIRECTION('center_axis',(0.,-1.,0.));
#11179=DIRECTION('ref_axis',(1.,0.,0.));
#11180=DIRECTION('center_axis',(0.,-1.,0.));
#11181=DIRECTION('ref_axis',(1.,0.,0.));
#11182=DIRECTION('',(0.,1.,0.));
#11183=DIRECTION('center_axis',(0.,-1.,0.));
#11184=DIRECTION('ref_axis',(0.,0.,-1.));
#11185=DIRECTION('center_axis',(0.,-1.,0.));
#11186=DIRECTION('ref_axis',(1.,0.,0.));
#11187=DIRECTION('center_axis',(0.,-1.,0.));
#11188=DIRECTION('ref_axis',(1.,0.,0.));
#11189=DIRECTION('',(0.,1.,0.));
#11190=DIRECTION('center_axis',(0.,1.,0.));
#11191=DIRECTION('ref_axis',(0.,0.,1.));
#11192=DIRECTION('center_axis',(0.,-1.,0.));
#11193=DIRECTION('ref_axis',(1.,0.,0.));
#11194=DIRECTION('center_axis',(0.,-1.,0.));
#11195=DIRECTION('ref_axis',(1.,0.,0.));
#11196=DIRECTION('center_axis',(0.,-1.,0.));
#11197=DIRECTION('ref_axis',(1.,0.,0.));
#11198=DIRECTION('center_axis',(0.,-1.,0.));
#11199=DIRECTION('ref_axis',(1.,0.,0.));
#11200=DIRECTION('',(0.,1.,0.));
#11201=DIRECTION('center_axis',(0.,-1.,0.));
#11202=DIRECTION('ref_axis',(0.,0.,-1.));
#11203=DIRECTION('center_axis',(0.,-1.,0.));
#11204=DIRECTION('ref_axis',(1.,0.,0.));
#11205=DIRECTION('center_axis',(0.,-1.,0.));
#11206=DIRECTION('ref_axis',(1.,0.,0.));
#11207=DIRECTION('',(0.,1.,0.));
#11208=DIRECTION('',(0.,0.,1.));
#11209=DIRECTION('',(1.,0.,0.));
#11210=DIRECTION('',(0.,0.,1.));
#11211=DIRECTION('',(1.,0.,0.));
#11212=DIRECTION('',(0.,0.,1.));
#11213=DIRECTION('',(1.,0.,0.));
#11214=DIRECTION('',(0.,0.,1.));
#11215=DIRECTION('',(1.,0.,0.));
#11216=DIRECTION('',(0.,0.,1.));
#11217=DIRECTION('',(1.,0.,0.));
#11218=DIRECTION('axis',(0.,0.,1.));
#11219=DIRECTION('refdir',(1.,0.,0.));
#11220=DIRECTION('axis',(0.,0.,1.));
#11221=DIRECTION('refdir',(1.,0.,0.));
#11222=DIRECTION('center_axis',(0.,1.,0.));
#11223=DIRECTION('ref_axis',(0.,0.,1.));
#11224=DIRECTION('center_axis',(0.,-1.,0.));
#11225=DIRECTION('ref_axis',(1.,0.,0.));
#11226=DIRECTION('',(-1.,0.,0.));
#11227=DIRECTION('',(0.,0.,-1.));
#11228=DIRECTION('',(1.,0.,0.));
#11229=DIRECTION('center_axis',(0.,0.,1.));
#11230=DIRECTION('ref_axis',(1.,0.,0.));
#11231=DIRECTION('',(0.,-1.,0.));
#11232=DIRECTION('',(0.,1.,0.));
#11233=DIRECTION('',(-1.,0.,0.));
#11234=DIRECTION('center_axis',(0.,-1.,0.));
#11235=DIRECTION('ref_axis',(0.,0.,-1.));
#11236=DIRECTION('center_axis',(0.,1.,0.));
#11237=DIRECTION('ref_axis',(1.,0.,0.));
#11238=DIRECTION('',(0.,0.,1.));
#11239=DIRECTION('',(1.,0.,0.));
#11240=DIRECTION('center_axis',(0.,0.,-1.));
#11241=DIRECTION('ref_axis',(-1.,0.,0.));
#11242=DIRECTION('',(0.,1.,0.));
#11243=DIRECTION('',(0.,1.,0.));
#11244=DIRECTION('center_axis',(1.,0.,0.));
#11245=DIRECTION('ref_axis',(0.,0.,-1.));
#11246=DIRECTION('center_axis',(0.,1.,0.));
#11247=DIRECTION('ref_axis',(0.,0.,1.));
#11248=DIRECTION('center_axis',(0.,-1.,0.));
#11249=DIRECTION('ref_axis',(1.,0.,0.));
#11250=DIRECTION('center_axis',(0.,-1.,0.));
#11251=DIRECTION('ref_axis',(1.,0.,0.));
#11252=DIRECTION('center_axis',(0.,-1.,0.));
#11253=DIRECTION('ref_axis',(1.,0.,0.));
#11254=DIRECTION('center_axis',(0.,-1.,0.));
#11255=DIRECTION('ref_axis',(1.,0.,0.));
#11256=DIRECTION('',(0.,1.,0.));
#11257=DIRECTION('center_axis',(0.,-1.,0.));
#11258=DIRECTION('ref_axis',(0.,0.,-1.));
#11259=DIRECTION('center_axis',(0.,-1.,0.));
#11260=DIRECTION('ref_axis',(1.,0.,0.));
#11261=DIRECTION('center_axis',(0.,-1.,0.));
#11262=DIRECTION('ref_axis',(1.,0.,0.));
#11263=DIRECTION('center_axis',(0.,-1.,0.));
#11264=DIRECTION('ref_axis',(1.,0.,0.));
#11265=DIRECTION('',(0.,1.,0.));
#11266=DIRECTION('center_axis',(0.,1.,0.));
#11267=DIRECTION('ref_axis',(0.,0.,1.));
#11268=DIRECTION('center_axis',(0.,-1.,0.));
#11269=DIRECTION('ref_axis',(1.,0.,0.));
#11270=DIRECTION('center_axis',(0.,-1.,0.));
#11271=DIRECTION('ref_axis',(1.,0.,0.));
#11272=DIRECTION('center_axis',(0.,-1.,0.));
#11273=DIRECTION('ref_axis',(1.,0.,0.));
#11274=DIRECTION('',(0.,1.,0.));
#11275=DIRECTION('center_axis',(0.,-1.,0.));
#11276=DIRECTION('ref_axis',(0.,0.,-1.));
#11277=DIRECTION('center_axis',(0.,-1.,0.));
#11278=DIRECTION('ref_axis',(1.,0.,0.));
#11279=DIRECTION('center_axis',(0.,-1.,0.));
#11280=DIRECTION('ref_axis',(1.,0.,0.));
#11281=DIRECTION('center_axis',(0.,-1.,0.));
#11282=DIRECTION('ref_axis',(1.,0.,0.));
#11283=DIRECTION('',(0.,1.,0.));
#11284=DIRECTION('center_axis',(0.,1.,0.));
#11285=DIRECTION('ref_axis',(0.,0.,1.));
#11286=DIRECTION('center_axis',(0.,-1.,0.));
#11287=DIRECTION('ref_axis',(1.,0.,0.));
#11288=DIRECTION('center_axis',(0.,-1.,0.));
#11289=DIRECTION('ref_axis',(1.,0.,0.));
#11290=DIRECTION('center_axis',(0.,-1.,0.));
#11291=DIRECTION('ref_axis',(1.,0.,0.));
#11292=DIRECTION('',(0.,1.,0.));
#11293=DIRECTION('center_axis',(0.,-1.,0.));
#11294=DIRECTION('ref_axis',(0.,0.,-1.));
#11295=DIRECTION('center_axis',(0.,-1.,0.));
#11296=DIRECTION('ref_axis',(1.,0.,0.));
#11297=DIRECTION('center_axis',(0.,-1.,0.));
#11298=DIRECTION('ref_axis',(1.,0.,0.));
#11299=DIRECTION('',(0.,1.,0.));
#11300=DIRECTION('axis',(0.,0.,1.));
#11301=DIRECTION('refdir',(1.,0.,0.));
#11302=DIRECTION('center_axis',(0.,1.,0.));
#11303=DIRECTION('ref_axis',(0.,0.,1.));
#11304=DIRECTION('center_axis',(0.,1.,0.));
#11305=DIRECTION('ref_axis',(1.,0.,0.));
#11306=DIRECTION('',(1.,0.,0.));
#11307=DIRECTION('center_axis',(0.,-1.,0.));
#11308=DIRECTION('ref_axis',(1.,0.,0.));
#11309=DIRECTION('',(-1.,0.,0.));
#11310=DIRECTION('center_axis',(0.,0.,-1.));
#11311=DIRECTION('ref_axis',(-1.,0.,0.));
#11312=DIRECTION('',(0.,-1.,0.));
#11313=DIRECTION('',(0.,1.,0.));
#11314=DIRECTION('',(1.,0.,0.));
#11315=DIRECTION('center_axis',(0.,-1.,0.));
#11316=DIRECTION('ref_axis',(0.,0.,-1.));
#11317=DIRECTION('center_axis',(0.,-1.,0.));
#11318=DIRECTION('ref_axis',(1.,0.,0.));
#11319=DIRECTION('center_axis',(0.,1.,0.));
#11320=DIRECTION('ref_axis',(1.,0.,0.));
#11321=DIRECTION('',(-1.,0.,0.));
#11322=DIRECTION('center_axis',(0.,0.,1.));
#11323=DIRECTION('ref_axis',(1.,0.,0.));
#11324=DIRECTION('',(0.,1.,0.));
#11325=DIRECTION('',(0.,-1.,0.));
#11326=DIRECTION('center_axis',(0.,1.,0.));
#11327=DIRECTION('ref_axis',(0.,0.,1.));
#11328=DIRECTION('center_axis',(0.,-1.,0.));
#11329=DIRECTION('ref_axis',(1.,0.,0.));
#11330=DIRECTION('center_axis',(0.,-1.,0.));
#11331=DIRECTION('ref_axis',(1.,0.,0.));
#11332=DIRECTION('center_axis',(0.,-1.,0.));
#11333=DIRECTION('ref_axis',(1.,0.,0.));
#11334=DIRECTION('center_axis',(0.,-1.,0.));
#11335=DIRECTION('ref_axis',(1.,0.,0.));
#11336=DIRECTION('',(0.,1.,0.));
#11337=DIRECTION('center_axis',(0.,-1.,0.));
#11338=DIRECTION('ref_axis',(0.,0.,-1.));
#11339=DIRECTION('center_axis',(0.,-1.,0.));
#11340=DIRECTION('ref_axis',(1.,0.,0.));
#11341=DIRECTION('center_axis',(0.,-1.,0.));
#11342=DIRECTION('ref_axis',(1.,0.,0.));
#11343=DIRECTION('',(0.,1.,0.));
#11344=DIRECTION('',(0.,0.,1.));
#11345=DIRECTION('',(1.,0.,0.));
#11346=DIRECTION('',(0.,0.,1.));
#11347=DIRECTION('',(1.,0.,0.));
#11348=DIRECTION('axis',(0.,0.,1.));
#11349=DIRECTION('refdir',(1.,0.,0.));
#11350=DIRECTION('center_axis',(0.866025403784439,0.,-0.5));
#11351=DIRECTION('ref_axis',(0.5,0.,0.866025403784439));
#11352=DIRECTION('',(-0.5,0.,-0.866025403784439));
#11353=DIRECTION('',(0.,-1.,0.));
#11354=DIRECTION('',(0.5,0.,0.866025403784439));
#11355=DIRECTION('',(0.,-1.,0.));
#11356=DIRECTION('center_axis',(1.60246890531964E-16,0.,-1.));
#11357=DIRECTION('ref_axis',(1.,0.,1.60246890531964E-16));
#11358=DIRECTION('',(-1.,0.,-1.60246890531964E-16));
#11359=DIRECTION('',(0.,-1.,0.));
#11360=DIRECTION('',(1.,0.,1.60246890531964E-16));
#11361=DIRECTION('center_axis',(-0.866025403784439,0.,-0.5));
#11362=DIRECTION('ref_axis',(0.5,0.,-0.866025403784439));
#11363=DIRECTION('',(-0.5,0.,0.866025403784439));
#11364=DIRECTION('',(0.,-1.,0.));
#11365=DIRECTION('',(0.5,0.,-0.866025403784439));
#11366=DIRECTION('center_axis',(-0.866025403784439,0.,0.5));
#11367=DIRECTION('ref_axis',(-0.5,0.,-0.866025403784439));
#11368=DIRECTION('',(0.5,0.,0.866025403784439));
#11369=DIRECTION('',(0.,-1.,0.));
#11370=DIRECTION('',(-0.5,0.,-0.866025403784439));
#11371=DIRECTION('center_axis',(-1.60246890531964E-16,0.,1.));
#11372=DIRECTION('ref_axis',(-1.,0.,-1.60246890531964E-16));
#11373=DIRECTION('',(1.,0.,1.60246890531964E-16));
#11374=DIRECTION('',(0.,-1.,0.));
#11375=DIRECTION('',(-1.,0.,-1.60246890531964E-16));
#11376=DIRECTION('center_axis',(0.866025403784439,0.,0.5));
#11377=DIRECTION('ref_axis',(-0.5,0.,0.866025403784439));
#11378=DIRECTION('',(0.5,0.,-0.866025403784439));
#11379=DIRECTION('',(-0.5,0.,0.866025403784439));
#11380=DIRECTION('center_axis',(0.,1.,0.));
#11381=DIRECTION('ref_axis',(1.,0.,0.));
#11382=DIRECTION('center_axis',(0.,-1.,0.));
#11383=DIRECTION('ref_axis',(0.,0.,-1.));
#11384=DIRECTION('center_axis',(0.,1.,0.));
#11385=DIRECTION('ref_axis',(1.,0.,0.));
#11386=DIRECTION('center_axis',(0.,1.,0.));
#11387=DIRECTION('ref_axis',(1.,0.,0.));
#11388=DIRECTION('center_axis',(0.,-1.,0.));
#11389=DIRECTION('ref_axis',(1.,0.,0.));
#11390=DIRECTION('center_axis',(0.,1.,0.));
#11391=DIRECTION('ref_axis',(1.,0.,0.));
#11392=DIRECTION('',(0.,-1.,0.));
#11393=DIRECTION('center_axis',(0.,1.,0.));
#11394=DIRECTION('ref_axis',(1.,0.,0.));
#11395=DIRECTION('center_axis',(0.,1.,0.));
#11396=DIRECTION('ref_axis',(1.,0.,0.));
#11397=DIRECTION('center_axis',(0.,1.,0.));
#11398=DIRECTION('ref_axis',(0.,0.,1.));
#11399=DIRECTION('center_axis',(0.,-1.,0.));
#11400=DIRECTION('ref_axis',(1.,0.,0.));
#11401=DIRECTION('center_axis',(0.,-1.,0.));
#11402=DIRECTION('ref_axis',(1.,0.,0.));
#11403=DIRECTION('center_axis',(0.,-1.,0.));
#11404=DIRECTION('ref_axis',(1.,0.,0.));
#11405=DIRECTION('',(0.707106781186547,0.707106781186548,8.65956056235493E-17));
#11406=DIRECTION('center_axis',(0.,-1.,0.));
#11407=DIRECTION('ref_axis',(1.,0.,0.));
#11408=DIRECTION('center_axis',(0.,-1.,0.));
#11409=DIRECTION('ref_axis',(1.,0.,0.));
#11410=DIRECTION('',(0.,1.,0.));
#11411=DIRECTION('center_axis',(0.,1.,0.));
#11412=DIRECTION('ref_axis',(1.,0.,0.));
#11413=DIRECTION('center_axis',(0.,-1.,0.));
#11414=DIRECTION('ref_axis',(1.,0.,0.));
#11415=DIRECTION('',(-0.707106781186547,0.707106781186548,-8.65956056235493E-17));
#11416=DIRECTION('center_axis',(0.,-1.,0.));
#11417=DIRECTION('ref_axis',(0.,0.,-1.));
#11418=DIRECTION('center_axis',(0.,-1.,0.));
#11419=DIRECTION('ref_axis',(1.,0.,0.));
#11420=DIRECTION('center_axis',(0.,1.,0.));
#11421=DIRECTION('ref_axis',(1.,0.,0.));
#11422=DIRECTION('center_axis',(0.,1.,0.));
#11423=DIRECTION('ref_axis',(1.,0.,0.));
#11424=DIRECTION('',(-0.447213595499958,0.894427190999916,-5.47678698264203E-17));
#11425=DIRECTION('center_axis',(0.,-1.,0.));
#11426=DIRECTION('ref_axis',(1.,0.,0.));
#11427=DIRECTION('center_axis',(0.,1.,0.));
#11428=DIRECTION('ref_axis',(1.,0.,0.));
#11429=DIRECTION('',(0.,1.,0.));
#11430=DIRECTION('center_axis',(0.,1.,0.));
#11431=DIRECTION('ref_axis',(1.,0.,0.));
#11432=DIRECTION('',(-0.707106781186547,0.707106781186548,-8.65956056235493E-17));
#11433=DIRECTION('axis',(0.,0.,1.));
#11434=DIRECTION('refdir',(1.,0.,0.));
#11435=DIRECTION('axis',(0.,0.,1.));
#11436=DIRECTION('refdir',(1.,0.,0.));
#11437=DIRECTION('center_axis',(0.,1.,0.));
#11438=DIRECTION('ref_axis',(1.,0.,0.));
#11439=DIRECTION('center_axis',(0.,1.,0.));
#11440=DIRECTION('ref_axis',(1.,0.,0.));
#11441=DIRECTION('',(0.,1.,0.));
#11442=DIRECTION('center_axis',(0.,-1.,0.));
#11443=DIRECTION('ref_axis',(1.,0.,0.));
#11444=DIRECTION('center_axis',(0.,1.,0.));
#11445=DIRECTION('ref_axis',(-0.46947156278589,0.,0.882947592858928));
#11446=DIRECTION('',(0.,-1.,0.));
#11447=DIRECTION('center_axis',(0.,1.,0.));
#11448=DIRECTION('ref_axis',(1.,0.,0.));
#11449=DIRECTION('',(0.,1.,0.));
#11450=DIRECTION('center_axis',(0.,1.,0.));
#11451=DIRECTION('ref_axis',(1.,0.,0.));
#11452=DIRECTION('center_axis',(0.,1.,0.));
#11453=DIRECTION('ref_axis',(1.,0.,0.));
#11454=DIRECTION('',(-0.469471562785891,0.,0.882947592858927));
#11455=DIRECTION('center_axis',(0.,1.,0.));
#11456=DIRECTION('ref_axis',(1.,0.,0.));
#11457=DIRECTION('center_axis',(0.,1.,0.));
#11458=DIRECTION('ref_axis',(1.,0.,0.));
#11459=DIRECTION('',(-0.469471562785891,0.,0.882947592858927));
#11460=DIRECTION('center_axis',(0.,1.,0.));
#11461=DIRECTION('ref_axis',(1.,0.,0.));
#11462=DIRECTION('',(0.469471562785891,0.,-0.882947592858927));
#11463=DIRECTION('center_axis',(0.,1.,0.));
#11464=DIRECTION('ref_axis',(1.,0.,0.));
#11465=DIRECTION('',(0.469471562785891,0.,-0.882947592858927));
#11466=DIRECTION('center_axis',(0.,-1.,0.));
#11467=DIRECTION('ref_axis',(1.,0.,0.));
#11468=DIRECTION('center_axis',(-0.882947592858927,0.,-0.469471562785891));
#11469=DIRECTION('ref_axis',(-0.469471562785891,0.,0.882947592858927));
#11470=DIRECTION('',(-0.469471562785891,0.,0.882947592858927));
#11471=DIRECTION('',(0.,1.,0.));
#11472=DIRECTION('center_axis',(0.,1.,0.));
#11473=DIRECTION('ref_axis',(0.,0.,1.));
#11474=DIRECTION('',(0.469471562785891,0.,-0.882947592858927));
#11475=DIRECTION('center_axis',(0.,1.,0.));
#11476=DIRECTION('ref_axis',(1.,0.,0.));
#11477=DIRECTION('center_axis',(0.882947592858927,0.,0.469471562785891));
#11478=DIRECTION('ref_axis',(0.469471562785891,0.,-0.882947592858927));
#11479=DIRECTION('',(0.,-1.,0.));
#11480=DIRECTION('center_axis',(0.,1.,0.));
#11481=DIRECTION('ref_axis',(0.46947156278589,0.,-0.882947592858927));
#11482=DIRECTION('',(0.,-1.,0.));
#11483=DIRECTION('center_axis',(0.,1.,0.));
#11484=DIRECTION('ref_axis',(1.,0.,0.));
#11485=DIRECTION('',(0.,1.,0.));
#11486=DIRECTION('center_axis',(0.882947592858927,0.,0.469471562785891));
#11487=DIRECTION('ref_axis',(0.469471562785891,0.,-0.882947592858927));
#11488=DIRECTION('',(0.469471562785891,0.,-0.882947592858927));
#11489=DIRECTION('',(0.,1.,0.));
#11490=DIRECTION('center_axis',(0.,1.,0.));
#11491=DIRECTION('ref_axis',(0.,0.,1.));
#11492=DIRECTION('',(-0.469471562785891,0.,0.882947592858927));
#11493=DIRECTION('center_axis',(0.,1.,0.));
#11494=DIRECTION('ref_axis',(1.,0.,0.));
#11495=DIRECTION('center_axis',(-0.882947592858927,0.,-0.469471562785891));
#11496=DIRECTION('ref_axis',(-0.469471562785891,0.,0.882947592858927));
#11497=DIRECTION('',(0.,-1.,0.));
#11498=DIRECTION('center_axis',(0.,1.,0.));
#11499=DIRECTION('ref_axis',(1.,0.,0.));
#11500=DIRECTION('center_axis',(0.,1.,0.));
#11501=DIRECTION('ref_axis',(1.,0.,0.));
#11502=DIRECTION('center_axis',(0.,1.,0.));
#11503=DIRECTION('ref_axis',(1.,0.,0.));
#11504=DIRECTION('center_axis',(0.,1.,0.));
#11505=DIRECTION('ref_axis',(1.,0.,0.));
#11506=DIRECTION('',(0.,-1.,0.));
#11507=DIRECTION('center_axis',(0.,1.,0.));
#11508=DIRECTION('ref_axis',(1.,0.,0.));
#11509=DIRECTION('center_axis',(0.,1.,0.));
#11510=DIRECTION('ref_axis',(1.,0.,0.));
#11511=DIRECTION('center_axis',(0.,1.,0.));
#11512=DIRECTION('ref_axis',(1.,0.,0.));
#11513=DIRECTION('center_axis',(0.,1.,0.));
#11514=DIRECTION('ref_axis',(1.,0.,0.));
#11515=DIRECTION('',(0.,-1.,0.));
#11516=DIRECTION('center_axis',(0.,1.,0.));
#11517=DIRECTION('ref_axis',(1.,0.,0.));
#11518=DIRECTION('',(0.,-1.,0.));
#11519=DIRECTION('center_axis',(0.,1.,0.));
#11520=DIRECTION('ref_axis',(1.,0.,0.));
#11521=DIRECTION('center_axis',(0.,1.,0.));
#11522=DIRECTION('ref_axis',(1.,0.,0.));
#11523=DIRECTION('center_axis',(0.,1.,0.));
#11524=DIRECTION('ref_axis',(1.,0.,0.));
#11525=DIRECTION('',(0.,-1.,0.));
#11526=DIRECTION('center_axis',(0.,1.,0.));
#11527=DIRECTION('ref_axis',(1.,0.,0.));
#11528=DIRECTION('center_axis',(0.,1.,0.));
#11529=DIRECTION('ref_axis',(1.,0.,0.));
#11530=DIRECTION('axis',(0.,0.,1.));
#11531=DIRECTION('refdir',(1.,0.,0.));
#11532=DIRECTION('center_axis',(0.,1.,0.));
#11533=DIRECTION('ref_axis',(1.,0.,0.));
#11534=DIRECTION('center_axis',(0.,-1.,0.));
#11535=DIRECTION('ref_axis',(1.,0.,0.));
#11536=DIRECTION('',(0.,-1.,0.));
#11537=DIRECTION('center_axis',(0.,-1.,0.));
#11538=DIRECTION('ref_axis',(1.,0.,0.));
#11539=DIRECTION('center_axis',(0.,1.,0.));
#11540=DIRECTION('ref_axis',(1.,0.,0.));
#11541=DIRECTION('center_axis',(0.,1.,0.));
#11542=DIRECTION('ref_axis',(1.,0.,0.));
#11543=DIRECTION('',(0.,-1.,0.));
#11544=DIRECTION('center_axis',(0.,1.,0.));
#11545=DIRECTION('ref_axis',(1.,0.,0.));
#11546=DIRECTION('center_axis',(0.,1.,0.));
#11547=DIRECTION('ref_axis',(1.,0.,0.));
#11548=DIRECTION('center_axis',(0.,1.,0.));
#11549=DIRECTION('ref_axis',(1.,0.,0.));
#11550=DIRECTION('axis',(0.,0.,1.));
#11551=DIRECTION('refdir',(1.,0.,0.));
#11552=DIRECTION('center_axis',(1.,0.,0.));
#11553=DIRECTION('ref_axis',(0.,0.,-1.));
#11554=DIRECTION('',(0.,1.,0.));
#11555=DIRECTION('center_axis',(1.,0.,0.));
#11556=DIRECTION('ref_axis',(0.,0.,-1.));
#11557=DIRECTION('center_axis',(1.,0.,0.));
#11558=DIRECTION('ref_axis',(0.,0.,-1.));
#11559=DIRECTION('center_axis',(1.,0.,0.));
#11560=DIRECTION('ref_axis',(0.,0.,-1.));
#11561=DIRECTION('',(1.,0.,0.));
#11562=DIRECTION('center_axis',(1.,0.,0.));
#11563=DIRECTION('ref_axis',(0.,0.,-1.));
#11564=DIRECTION('center_axis',(1.,0.,0.));
#11565=DIRECTION('ref_axis',(0.,0.,-1.));
#11566=DIRECTION('',(0.,-1.,0.));
#11567=DIRECTION('center_axis',(0.,1.,0.));
#11568=DIRECTION('ref_axis',(1.,0.,0.));
#11569=DIRECTION('center_axis',(0.,-1.,0.));
#11570=DIRECTION('ref_axis',(1.,0.,0.));
#11571=DIRECTION('',(0.,-1.,0.));
#11572=DIRECTION('center_axis',(0.,-1.,0.));
#11573=DIRECTION('ref_axis',(1.,0.,0.));
#11574=DIRECTION('center_axis',(0.,1.,0.));
#11575=DIRECTION('ref_axis',(1.,0.,0.));
#11576=DIRECTION('center_axis',(0.,1.,0.));
#11577=DIRECTION('ref_axis',(1.,0.,0.));
#11578=DIRECTION('',(0.,-1.,0.));
#11579=DIRECTION('center_axis',(0.,1.,0.));
#11580=DIRECTION('ref_axis',(1.,0.,0.));
#11581=DIRECTION('center_axis',(0.,1.,0.));
#11582=DIRECTION('ref_axis',(1.,0.,0.));
#11583=DIRECTION('center_axis',(0.,1.,0.));
#11584=DIRECTION('ref_axis',(1.,0.,0.));
#11585=DIRECTION('axis',(0.,0.,1.));
#11586=DIRECTION('refdir',(1.,0.,0.));
#11587=DIRECTION('center_axis',(0.,1.,0.));
#11588=DIRECTION('ref_axis',(1.,0.,0.));
#11589=DIRECTION('center_axis',(0.,1.,0.));
#11590=DIRECTION('ref_axis',(1.,0.,0.));
#11591=DIRECTION('',(0.,1.,0.));
#11592=DIRECTION('center_axis',(0.,-1.,0.));
#11593=DIRECTION('ref_axis',(1.,0.,0.));
#11594=DIRECTION('center_axis',(0.,1.,0.));
#11595=DIRECTION('ref_axis',(1.,0.,0.));
#11596=DIRECTION('center_axis',(0.,1.,0.));
#11597=DIRECTION('ref_axis',(1.,0.,0.));
#11598=DIRECTION('center_axis',(0.,1.,0.));
#11599=DIRECTION('ref_axis',(1.,0.,0.));
#11600=DIRECTION('',(0.,1.,0.));
#11601=DIRECTION('center_axis',(0.,1.,0.));
#11602=DIRECTION('ref_axis',(1.,0.,0.));
#11603=DIRECTION('center_axis',(0.,1.,0.));
#11604=DIRECTION('ref_axis',(1.,0.,0.));
#11605=DIRECTION('center_axis',(0.,1.,0.));
#11606=DIRECTION('ref_axis',(1.,0.,0.));
#11607=DIRECTION('center_axis',(0.,1.,0.));
#11608=DIRECTION('ref_axis',(1.,0.,0.));
#11609=DIRECTION('center_axis',(0.,1.,0.));
#11610=DIRECTION('ref_axis',(1.,0.,0.));
#11611=DIRECTION('center_axis',(0.,1.,0.));
#11612=DIRECTION('ref_axis',(1.,0.,0.));
#11613=DIRECTION('center_axis',(0.,1.,0.));
#11614=DIRECTION('ref_axis',(1.,0.,0.));
#11615=DIRECTION('center_axis',(0.,-1.,0.));
#11616=DIRECTION('ref_axis',(1.,0.,0.));
#11617=DIRECTION('center_axis',(0.,1.,0.));
#11618=DIRECTION('ref_axis',(1.,0.,0.));
#11619=DIRECTION('',(0.,-1.,0.));
#11620=DIRECTION('center_axis',(0.,1.,0.));
#11621=DIRECTION('ref_axis',(1.,0.,0.));
#11622=DIRECTION('',(0.,-1.,0.));
#11623=DIRECTION('center_axis',(0.,1.,0.));
#11624=DIRECTION('ref_axis',(1.,0.,0.));
#11625=DIRECTION('center_axis',(0.,1.,0.));
#11626=DIRECTION('ref_axis',(1.,0.,0.));
#11627=DIRECTION('center_axis',(0.,1.,0.));
#11628=DIRECTION('ref_axis',(1.,0.,0.));
#11629=DIRECTION('',(0.,-1.,0.));
#11630=DIRECTION('center_axis',(0.,1.,0.));
#11631=DIRECTION('ref_axis',(1.,0.,0.));
#11632=DIRECTION('center_axis',(0.,1.,0.));
#11633=DIRECTION('ref_axis',(1.,0.,0.));
#11634=DIRECTION('axis',(0.,0.,1.));
#11635=DIRECTION('refdir',(1.,0.,0.));
#11636=DIRECTION('center_axis',(0.,1.,0.));
#11637=DIRECTION('ref_axis',(1.,0.,0.));
#11638=DIRECTION('center_axis',(0.,-1.,0.));
#11639=DIRECTION('ref_axis',(1.,0.,0.));
#11640=DIRECTION('',(0.,-1.,0.));
#11641=DIRECTION('center_axis',(0.,-1.,0.));
#11642=DIRECTION('ref_axis',(1.,0.,0.));
#11643=DIRECTION('center_axis',(0.,1.,0.));
#11644=DIRECTION('ref_axis',(1.,0.,0.));
#11645=DIRECTION('center_axis',(0.,1.,0.));
#11646=DIRECTION('ref_axis',(1.,0.,0.));
#11647=DIRECTION('',(0.,-1.,0.));
#11648=DIRECTION('center_axis',(0.,1.,0.));
#11649=DIRECTION('ref_axis',(1.,0.,0.));
#11650=DIRECTION('center_axis',(0.,1.,0.));
#11651=DIRECTION('ref_axis',(1.,0.,0.));
#11652=DIRECTION('center_axis',(0.,1.,0.));
#11653=DIRECTION('ref_axis',(1.,0.,0.));
#11654=DIRECTION('axis',(0.,0.,1.));
#11655=DIRECTION('refdir',(1.,0.,0.));
#11656=DIRECTION('center_axis',(0.,1.,0.));
#11657=DIRECTION('ref_axis',(1.,0.,0.));
#11658=DIRECTION('center_axis',(0.,-1.,0.));
#11659=DIRECTION('ref_axis',(1.,0.,0.));
#11660=DIRECTION('',(0.,-1.,0.));
#11661=DIRECTION('center_axis',(0.,-1.,0.));
#11662=DIRECTION('ref_axis',(1.,0.,0.));
#11663=DIRECTION('center_axis',(0.,1.,0.));
#11664=DIRECTION('ref_axis',(1.,0.,0.));
#11665=DIRECTION('center_axis',(0.,1.,0.));
#11666=DIRECTION('ref_axis',(1.,0.,0.));
#11667=DIRECTION('',(0.,-1.,0.));
#11668=DIRECTION('center_axis',(0.,1.,0.));
#11669=DIRECTION('ref_axis',(1.,0.,0.));
#11670=DIRECTION('center_axis',(0.,1.,0.));
#11671=DIRECTION('ref_axis',(1.,0.,0.));
#11672=DIRECTION('center_axis',(0.,1.,0.));
#11673=DIRECTION('ref_axis',(1.,0.,0.));
#11674=DIRECTION('axis',(0.,0.,1.));
#11675=DIRECTION('refdir',(1.,0.,0.));
#11676=DIRECTION('center_axis',(0.,1.,0.));
#11677=DIRECTION('ref_axis',(1.,0.,0.));
#11678=DIRECTION('center_axis',(0.,-1.,0.));
#11679=DIRECTION('ref_axis',(1.,0.,0.));
#11680=DIRECTION('',(0.,-1.,0.));
#11681=DIRECTION('center_axis',(0.,-1.,0.));
#11682=DIRECTION('ref_axis',(1.,0.,0.));
#11683=DIRECTION('center_axis',(0.,1.,0.));
#11684=DIRECTION('ref_axis',(1.,0.,0.));
#11685=DIRECTION('center_axis',(0.,1.,0.));
#11686=DIRECTION('ref_axis',(1.,0.,0.));
#11687=DIRECTION('',(0.,-1.,0.));
#11688=DIRECTION('center_axis',(0.,1.,0.));
#11689=DIRECTION('ref_axis',(1.,0.,0.));
#11690=DIRECTION('center_axis',(0.,1.,0.));
#11691=DIRECTION('ref_axis',(1.,0.,0.));
#11692=DIRECTION('center_axis',(0.,1.,0.));
#11693=DIRECTION('ref_axis',(1.,0.,0.));
#11694=DIRECTION('axis',(0.,0.,1.));
#11695=DIRECTION('refdir',(1.,0.,0.));
#11696=DIRECTION('center_axis',(0.,1.,0.));
#11697=DIRECTION('ref_axis',(1.,0.,0.));
#11698=DIRECTION('center_axis',(0.,-1.,0.));
#11699=DIRECTION('ref_axis',(1.,0.,0.));
#11700=DIRECTION('',(0.,-1.,0.));
#11701=DIRECTION('center_axis',(0.,-1.,0.));
#11702=DIRECTION('ref_axis',(1.,0.,0.));
#11703=DIRECTION('center_axis',(0.,1.,0.));
#11704=DIRECTION('ref_axis',(1.,0.,0.));
#11705=DIRECTION('center_axis',(0.,1.,0.));
#11706=DIRECTION('ref_axis',(1.,0.,0.));
#11707=DIRECTION('',(0.,-1.,0.));
#11708=DIRECTION('center_axis',(0.,1.,0.));
#11709=DIRECTION('ref_axis',(1.,0.,0.));
#11710=DIRECTION('center_axis',(0.,1.,0.));
#11711=DIRECTION('ref_axis',(1.,0.,0.));
#11712=DIRECTION('center_axis',(0.,1.,0.));
#11713=DIRECTION('ref_axis',(1.,0.,0.));
#11714=DIRECTION('axis',(0.,0.,1.));
#11715=DIRECTION('refdir',(1.,0.,0.));
#11716=DIRECTION('center_axis',(0.,1.,0.));
#11717=DIRECTION('ref_axis',(1.,0.,0.));
#11718=DIRECTION('center_axis',(0.,1.,0.));
#11719=DIRECTION('ref_axis',(1.,0.,0.));
#11720=DIRECTION('center_axis',(0.866025403784439,0.,-0.5));
#11721=DIRECTION('ref_axis',(0.5,0.,0.866025403784439));
#11722=DIRECTION('',(0.5,0.,0.866025403784439));
#11723=DIRECTION('',(0.,-1.,0.));
#11724=DIRECTION('',(0.5,0.,0.866025403784439));
#11725=DIRECTION('',(0.,-1.,0.));
#11726=DIRECTION('center_axis',(1.20185167898973E-16,0.,-1.));
#11727=DIRECTION('ref_axis',(1.,0.,1.20185167898973E-16));
#11728=DIRECTION('',(1.,0.,1.20185167898973E-16));
#11729=DIRECTION('',(0.,-1.,0.));
#11730=DIRECTION('',(1.,0.,1.20185167898973E-16));
#11731=DIRECTION('center_axis',(-0.866025403784439,0.,-0.5));
#11732=DIRECTION('ref_axis',(0.5,0.,-0.866025403784439));
#11733=DIRECTION('',(0.5,0.,-0.866025403784439));
#11734=DIRECTION('',(0.,-1.,0.));
#11735=DIRECTION('',(0.5,0.,-0.866025403784439));
#11736=DIRECTION('center_axis',(-0.866025403784439,0.,0.5));
#11737=DIRECTION('ref_axis',(-0.5,0.,-0.866025403784439));
#11738=DIRECTION('',(-0.5,0.,-0.866025403784439));
#11739=DIRECTION('',(0.,-1.,0.));
#11740=DIRECTION('',(-0.5,0.,-0.866025403784439));
#11741=DIRECTION('center_axis',(-2.40370335797945E-16,0.,1.));
#11742=DIRECTION('ref_axis',(-1.,0.,-2.40370335797945E-16));
#11743=DIRECTION('',(-1.,0.,-2.40370335797945E-16));
#11744=DIRECTION('',(0.,-1.,0.));
#11745=DIRECTION('',(-1.,0.,-2.40370335797945E-16));
#11746=DIRECTION('center_axis',(0.866025403784439,0.,0.5));
#11747=DIRECTION('ref_axis',(-0.5,0.,0.866025403784439));
#11748=DIRECTION('',(-0.5,0.,0.866025403784439));
#11749=DIRECTION('',(-0.5,0.,0.866025403784439));
#11750=DIRECTION('center_axis',(0.,-1.,0.));
#11751=DIRECTION('ref_axis',(0.,0.,-1.));
#11752=DIRECTION('center_axis',(0.,1.,0.));
#11753=DIRECTION('ref_axis',(0.,0.,1.));
#11754=DIRECTION('center_axis',(0.,-1.,0.));
#11755=DIRECTION('ref_axis',(1.,0.,0.));
#11756=DIRECTION('center_axis',(0.,-1.,0.));
#11757=DIRECTION('ref_axis',(1.,0.,0.));
#11758=DIRECTION('center_axis',(0.,-1.,0.));
#11759=DIRECTION('ref_axis',(1.,0.,0.));
#11760=DIRECTION('',(0.707106781186548,0.707106781186547,8.65956056235494E-17));
#11761=DIRECTION('center_axis',(0.,-1.,0.));
#11762=DIRECTION('ref_axis',(1.,0.,0.));
#11763=DIRECTION('',(0.,1.,0.));
#11764=DIRECTION('axis',(0.,0.,1.));
#11765=DIRECTION('refdir',(1.,0.,0.));
#11766=DIRECTION('center_axis',(0.866025403784439,0.,-0.5));
#11767=DIRECTION('ref_axis',(0.5,0.,0.866025403784439));
#11768=DIRECTION('',(-0.5,0.,-0.866025403784439));
#11769=DIRECTION('',(0.,-1.,0.));
#11770=DIRECTION('',(0.5,0.,0.866025403784439));
#11771=DIRECTION('',(0.,-1.,0.));
#11772=DIRECTION('center_axis',(1.60246890531964E-16,0.,-1.));
#11773=DIRECTION('ref_axis',(1.,0.,1.60246890531964E-16));
#11774=DIRECTION('',(-1.,0.,-1.60246890531964E-16));
#11775=DIRECTION('',(0.,-1.,0.));
#11776=DIRECTION('',(1.,0.,1.60246890531964E-16));
#11777=DIRECTION('center_axis',(-0.866025403784439,0.,-0.5));
#11778=DIRECTION('ref_axis',(0.5,0.,-0.866025403784439));
#11779=DIRECTION('',(-0.5,0.,0.866025403784439));
#11780=DIRECTION('',(0.,-1.,0.));
#11781=DIRECTION('',(0.5,0.,-0.866025403784439));
#11782=DIRECTION('center_axis',(-0.866025403784439,0.,0.5));
#11783=DIRECTION('ref_axis',(-0.5,0.,-0.866025403784439));
#11784=DIRECTION('',(0.5,0.,0.866025403784439));
#11785=DIRECTION('',(0.,-1.,0.));
#11786=DIRECTION('',(-0.5,0.,-0.866025403784439));
#11787=DIRECTION('center_axis',(-1.60246890531964E-16,0.,1.));
#11788=DIRECTION('ref_axis',(-1.,0.,-1.60246890531964E-16));
#11789=DIRECTION('',(1.,0.,1.60246890531964E-16));
#11790=DIRECTION('',(0.,-1.,0.));
#11791=DIRECTION('',(-1.,0.,-1.60246890531964E-16));
#11792=DIRECTION('center_axis',(0.866025403784439,0.,0.5));
#11793=DIRECTION('ref_axis',(-0.5,0.,0.866025403784439));
#11794=DIRECTION('',(0.5,0.,-0.866025403784439));
#11795=DIRECTION('',(-0.5,0.,0.866025403784439));
#11796=DIRECTION('center_axis',(0.,1.,0.));
#11797=DIRECTION('ref_axis',(1.,0.,0.));
#11798=DIRECTION('center_axis',(0.,-1.,0.));
#11799=DIRECTION('ref_axis',(0.,0.,-1.));
#11800=DIRECTION('center_axis',(0.,1.,0.));
#11801=DIRECTION('ref_axis',(1.,0.,0.));
#11802=DIRECTION('center_axis',(0.,1.,0.));
#11803=DIRECTION('ref_axis',(1.,0.,0.));
#11804=DIRECTION('center_axis',(0.,1.,0.));
#11805=DIRECTION('ref_axis',(0.,0.,1.));
#11806=DIRECTION('center_axis',(0.,-1.,0.));
#11807=DIRECTION('ref_axis',(1.,0.,0.));
#11808=DIRECTION('center_axis',(0.,-1.,0.));
#11809=DIRECTION('ref_axis',(1.,0.,0.));
#11810=DIRECTION('center_axis',(0.,-1.,0.));
#11811=DIRECTION('ref_axis',(1.,0.,0.));
#11812=DIRECTION('',(0.707106781186547,0.707106781186548,8.65956056235493E-17));
#11813=DIRECTION('center_axis',(0.,-1.,0.));
#11814=DIRECTION('ref_axis',(1.,0.,0.));
#11815=DIRECTION('center_axis',(0.,-1.,0.));
#11816=DIRECTION('ref_axis',(1.,0.,0.));
#11817=DIRECTION('',(0.,1.,0.));
#11818=DIRECTION('center_axis',(0.,1.,0.));
#11819=DIRECTION('ref_axis',(1.,0.,0.));
#11820=DIRECTION('center_axis',(0.,-1.,0.));
#11821=DIRECTION('ref_axis',(1.,0.,0.));
#11822=DIRECTION('',(-0.707106781186547,0.707106781186548,-8.65956056235493E-17));
#11823=DIRECTION('center_axis',(0.,-1.,0.));
#11824=DIRECTION('ref_axis',(0.,0.,-1.));
#11825=DIRECTION('center_axis',(0.,-1.,0.));
#11826=DIRECTION('ref_axis',(1.,0.,0.));
#11827=DIRECTION('center_axis',(0.,1.,0.));
#11828=DIRECTION('ref_axis',(1.,0.,0.));
#11829=DIRECTION('center_axis',(0.,1.,0.));
#11830=DIRECTION('ref_axis',(1.,0.,0.));
#11831=DIRECTION('',(-0.447213595499958,0.894427190999916,-5.47678698264203E-17));
#11832=DIRECTION('center_axis',(0.,-1.,0.));
#11833=DIRECTION('ref_axis',(1.,0.,0.));
#11834=DIRECTION('',(0.,1.,0.));
#11835=DIRECTION('axis',(0.,0.,1.));
#11836=DIRECTION('refdir',(1.,0.,0.));
#11837=DIRECTION('center_axis',(0.,1.,0.));
#11838=DIRECTION('ref_axis',(0.,0.,1.));
#11839=DIRECTION('center_axis',(0.,-1.,0.));
#11840=DIRECTION('ref_axis',(1.,0.,0.));
#11841=DIRECTION('center_axis',(0.,-1.,0.));
#11842=DIRECTION('ref_axis',(1.,0.,0.));
#11843=DIRECTION('center_axis',(0.,-1.,0.));
#11844=DIRECTION('ref_axis',(1.,0.,0.));
#11845=DIRECTION('',(0.707106781186547,0.707106781186548,8.65956056235493E-17));
#11846=DIRECTION('center_axis',(0.,-1.,0.));
#11847=DIRECTION('ref_axis',(1.,0.,0.));
#11848=DIRECTION('center_axis',(0.,-1.,0.));
#11849=DIRECTION('ref_axis',(1.,0.,0.));
#11850=DIRECTION('',(0.,1.,0.));
#11851=DIRECTION('center_axis',(0.,1.,0.));
#11852=DIRECTION('ref_axis',(1.,0.,0.));
#11853=DIRECTION('center_axis',(0.,-1.,0.));
#11854=DIRECTION('ref_axis',(1.,0.,0.));
#11855=DIRECTION('',(-0.707106781186547,0.707106781186548,-8.65956056235493E-17));
#11856=DIRECTION('center_axis',(0.,-1.,0.));
#11857=DIRECTION('ref_axis',(0.,0.,-1.));
#11858=DIRECTION('center_axis',(0.,-1.,0.));
#11859=DIRECTION('ref_axis',(1.,0.,0.));
#11860=DIRECTION('center_axis',(0.,1.,0.));
#11861=DIRECTION('ref_axis',(1.,0.,0.));
#11862=DIRECTION('center_axis',(0.,1.,0.));
#11863=DIRECTION('ref_axis',(1.,0.,0.));
#11864=DIRECTION('',(-0.447213595499958,0.894427190999916,-5.47678698264203E-17));
#11865=DIRECTION('center_axis',(0.,-1.,0.));
#11866=DIRECTION('ref_axis',(1.,0.,0.));
#11867=DIRECTION('center_axis',(0.,1.,0.));
#11868=DIRECTION('ref_axis',(1.,0.,0.));
#11869=DIRECTION('',(0.,1.,0.));
#11870=DIRECTION('center_axis',(0.,1.,0.));
#11871=DIRECTION('ref_axis',(1.,0.,0.));
#11872=DIRECTION('center_axis',(0.,-1.,0.));
#11873=DIRECTION('ref_axis',(1.,0.,0.));
#11874=DIRECTION('',(-0.707106781186547,0.707106781186548,-8.65956056235493E-17));
#11875=DIRECTION('center_axis',(0.,-1.,0.));
#11876=DIRECTION('ref_axis',(0.,0.,-1.));
#11877=DIRECTION('center_axis',(0.866025403784439,0.,-0.5));
#11878=DIRECTION('ref_axis',(0.5,0.,0.866025403784439));
#11879=DIRECTION('',(-0.5,0.,-0.866025403784439));
#11880=DIRECTION('',(0.,-1.,0.));
#11881=DIRECTION('',(0.5,0.,0.866025403784439));
#11882=DIRECTION('',(0.,-1.,0.));
#11883=DIRECTION('center_axis',(1.60246890531964E-16,0.,-1.));
#11884=DIRECTION('ref_axis',(1.,0.,1.60246890531964E-16));
#11885=DIRECTION('',(-1.,0.,-1.60246890531964E-16));
#11886=DIRECTION('',(0.,-1.,0.));
#11887=DIRECTION('',(1.,0.,1.60246890531964E-16));
#11888=DIRECTION('center_axis',(-0.866025403784439,0.,-0.5));
#11889=DIRECTION('ref_axis',(0.5,0.,-0.866025403784439));
#11890=DIRECTION('',(-0.5,0.,0.866025403784439));
#11891=DIRECTION('',(0.,-1.,0.));
#11892=DIRECTION('',(0.5,0.,-0.866025403784439));
#11893=DIRECTION('center_axis',(-0.866025403784439,0.,0.5));
#11894=DIRECTION('ref_axis',(-0.5,0.,-0.866025403784439));
#11895=DIRECTION('',(0.5,0.,0.866025403784439));
#11896=DIRECTION('',(0.,-1.,0.));
#11897=DIRECTION('',(-0.5,0.,-0.866025403784439));
#11898=DIRECTION('center_axis',(-1.60246890531964E-16,0.,1.));
#11899=DIRECTION('ref_axis',(-1.,0.,-1.60246890531964E-16));
#11900=DIRECTION('',(1.,0.,1.60246890531964E-16));
#11901=DIRECTION('',(0.,-1.,0.));
#11902=DIRECTION('',(-1.,0.,-1.60246890531964E-16));
#11903=DIRECTION('center_axis',(0.866025403784439,0.,0.5));
#11904=DIRECTION('ref_axis',(-0.5,0.,0.866025403784439));
#11905=DIRECTION('',(0.5,0.,-0.866025403784439));
#11906=DIRECTION('',(-0.5,0.,0.866025403784439));
#11907=DIRECTION('center_axis',(0.,1.,0.));
#11908=DIRECTION('ref_axis',(1.,0.,0.));
#11909=DIRECTION('center_axis',(0.,-1.,0.));
#11910=DIRECTION('ref_axis',(0.,0.,-1.));
#11911=DIRECTION('',(0.,0.,1.));
#11912=DIRECTION('',(1.,0.,0.));
#11913=DIRECTION('',(0.,0.,1.));
#11914=DIRECTION('',(1.,0.,0.));
#11915=DIRECTION('',(0.,0.,1.));
#11916=DIRECTION('',(1.,0.,0.));
#11917=DIRECTION('',(0.,0.,1.));
#11918=DIRECTION('',(1.,0.,0.));
#11919=DIRECTION('',(0.,0.,1.));
#11920=DIRECTION('',(1.,0.,0.));
#11921=DIRECTION('',(0.,0.,1.));
#11922=DIRECTION('',(1.,0.,0.));
#11923=DIRECTION('',(0.,0.,1.));
#11924=DIRECTION('',(1.,0.,0.));
#11925=DIRECTION('',(0.,0.,1.));
#11926=DIRECTION('',(1.,0.,0.));
#11927=DIRECTION('',(0.,0.,1.));
#11928=DIRECTION('',(1.,0.,0.));
#11929=DIRECTION('',(0.,0.,1.));
#11930=DIRECTION('',(1.,0.,0.));
#11931=DIRECTION('',(0.,0.,1.));
#11932=DIRECTION('',(1.,0.,0.));
#11933=DIRECTION('',(0.,0.,1.));
#11934=DIRECTION('',(1.,0.,0.));
#11935=DIRECTION('',(0.,0.,1.));
#11936=DIRECTION('',(1.,0.,0.));
#11937=DIRECTION('',(0.,0.,1.));
#11938=DIRECTION('',(1.,0.,0.));
#11939=DIRECTION('',(0.,-1.,2.22044604925031E-16));
#11940=DIRECTION('',(1.,0.,0.));
#11941=DIRECTION('',(0.,-1.22464679914735E-16,-1.));
#11942=DIRECTION('',(1.,0.,0.));
#11943=DIRECTION('',(0.,1.,2.22044604925031E-16));
#11944=DIRECTION('',(1.,0.,0.));
#11945=DIRECTION('',(0.,1.,2.22044604925031E-16));
#11946=DIRECTION('',(1.,0.,0.));
#11947=DIRECTION('',(0.,0.,1.));
#11948=DIRECTION('',(1.,0.,0.));
#11949=DIRECTION('',(0.,-1.,2.22044604925031E-16));
#11950=DIRECTION('',(1.,0.,0.));
#11951=DIRECTION('',(0.,-1.22464679914735E-16,-1.));
#11952=DIRECTION('',(1.,0.,0.));
#11953=DIRECTION('',(0.,1.,2.22044604925031E-16));
#11954=DIRECTION('',(1.,0.,0.));
#11955=DIRECTION('',(0.,1.,2.22044604925031E-16));
#11956=DIRECTION('',(1.,0.,0.));
#11957=DIRECTION('',(0.,0.,1.));
#11958=DIRECTION('',(1.,0.,0.));
#11959=DIRECTION('',(0.,0.,1.));
#11960=DIRECTION('',(1.,0.,0.));
#11961=DIRECTION('',(0.,-1.,2.22044604925031E-16));
#11962=DIRECTION('',(1.,0.,0.));
#11963=DIRECTION('',(0.,-1.22464679914735E-16,-1.));
#11964=DIRECTION('',(1.,0.,0.));
#11965=DIRECTION('',(0.,1.,2.22044604925031E-16));
#11966=DIRECTION('',(1.,0.,0.));
#11967=DIRECTION('',(0.,1.,2.22044604925031E-16));
#11968=DIRECTION('',(1.,0.,0.));
#11969=DIRECTION('',(0.,0.,1.));
#11970=DIRECTION('',(1.,0.,0.));
#11971=DIRECTION('',(0.,-1.,2.22044604925031E-16));
#11972=DIRECTION('',(1.,0.,0.));
#11973=DIRECTION('',(0.,-1.22464679914735E-16,-1.));
#11974=DIRECTION('',(1.,0.,0.));
#11975=DIRECTION('',(0.,1.,2.22044604925031E-16));
#11976=DIRECTION('',(1.,0.,0.));
#11977=DIRECTION('',(0.,1.,2.22044604925031E-16));
#11978=DIRECTION('',(1.,0.,0.));
#11979=DIRECTION('',(0.,-1.,2.22044604925031E-16));
#11980=DIRECTION('',(1.,0.,0.));
#11981=DIRECTION('',(0.,-1.,2.22044604925031E-16));
#11982=DIRECTION('',(1.,0.,0.));
#11983=DIRECTION('',(0.,-1.,2.22044604925031E-16));
#11984=DIRECTION('',(1.,0.,0.));
#11985=DIRECTION('',(0.,-1.,2.22044604925031E-16));
#11986=DIRECTION('',(1.,0.,0.));
#11987=DIRECTION('',(0.,0.,1.));
#11988=DIRECTION('',(1.,0.,0.));
#11989=DIRECTION('',(0.,-1.,2.22044604925031E-16));
#11990=DIRECTION('',(1.,0.,0.));
#11991=DIRECTION('',(0.,0.,1.));
#11992=DIRECTION('',(-1.,1.22464679914735E-16,0.));
#11993=DIRECTION('',(0.,0.,1.));
#11994=DIRECTION('',(-1.,1.22464679914735E-16,0.));
#11995=DIRECTION('',(0.,0.,1.));
#11996=DIRECTION('',(-1.,1.22464679914735E-16,0.));
#11997=DIRECTION('',(0.,0.,1.));
#11998=DIRECTION('',(-1.,1.22464679914735E-16,0.));
#11999=DIRECTION('',(0.,0.,1.));
#12000=DIRECTION('',(1.,0.,0.));
#12001=DIRECTION('',(0.,0.,1.));
#12002=DIRECTION('',(1.,0.,0.));
#12003=DIRECTION('',(0.,0.,1.));
#12004=DIRECTION('',(1.,0.,0.));
#12005=DIRECTION('',(0.,0.,1.));
#12006=DIRECTION('',(1.,0.,0.));
#12007=DIRECTION('',(0.,-1.,2.22044604925031E-16));
#12008=DIRECTION('',(1.,0.,0.));
#12009=DIRECTION('',(0.,-1.,2.22044604925031E-16));
#12010=DIRECTION('',(1.,0.,0.));
#12011=DIRECTION('',(0.,-1.,2.22044604925031E-16));
#12012=DIRECTION('',(1.,0.,0.));
#12013=DIRECTION('',(0.,-1.,2.22044604925031E-16));
#12014=DIRECTION('',(1.,0.,0.));
#12015=DIRECTION('',(0.,1.,2.22044604925031E-16));
#12016=DIRECTION('',(1.,0.,0.));
#12017=DIRECTION('',(0.,1.,2.22044604925031E-16));
#12018=DIRECTION('',(1.,0.,0.));
#12019=DIRECTION('',(0.,1.,2.22044604925031E-16));
#12020=DIRECTION('',(1.,0.,0.));
#12021=DIRECTION('',(0.,1.,2.22044604925031E-16));
#12022=DIRECTION('',(1.,0.,0.));
#12023=DIRECTION('',(0.,0.,1.));
#12024=DIRECTION('',(1.,0.,0.));
#12025=DIRECTION('',(0.,0.,1.));
#12026=DIRECTION('',(1.,0.,0.));
#12027=DIRECTION('',(0.,0.,1.));
#12028=DIRECTION('',(1.,0.,0.));
#12029=DIRECTION('',(0.,0.,1.));
#12030=DIRECTION('',(1.,0.,0.));
#12031=DIRECTION('',(0.,0.,1.));
#12032=DIRECTION('',(1.,0.,0.));
#12033=DIRECTION('',(0.,0.,1.));
#12034=DIRECTION('',(1.,0.,0.));
#12035=DIRECTION('',(0.,0.,1.));
#12036=DIRECTION('',(1.,0.,0.));
#12037=DIRECTION('',(0.,0.,1.));
#12038=DIRECTION('',(1.,0.,0.));
#12039=DIRECTION('',(0.,0.,1.));
#12040=DIRECTION('',(1.,0.,0.));
#12041=DIRECTION('',(0.,0.,1.));
#12042=DIRECTION('',(2.22044604925031E-16,-1.,0.));
#12043=DIRECTION('',(0.,0.,1.));
#12044=DIRECTION('',(-1.,1.22464679914735E-16,0.));
#12045=DIRECTION('',(0.,0.,1.));
#12046=DIRECTION('',(1.,0.,0.));
#12047=DIRECTION('axis',(0.,0.,1.));
#12048=DIRECTION('refdir',(1.,0.,0.));
#12049=DIRECTION('axis',(0.,0.,1.));
#12050=DIRECTION('refdir',(1.,0.,0.));
#12051=DIRECTION('center_axis',(0.,1.,0.));
#12052=DIRECTION('ref_axis',(1.,0.,0.));
#12053=DIRECTION('center_axis',(0.,1.,0.));
#12054=DIRECTION('ref_axis',(1.,0.,0.));
#12055=DIRECTION('',(0.,1.,0.));
#12056=DIRECTION('center_axis',(0.,-1.,0.));
#12057=DIRECTION('ref_axis',(1.,0.,0.));
#12058=DIRECTION('center_axis',(0.,1.,0.));
#12059=DIRECTION('ref_axis',(1.,0.,0.));
#12060=DIRECTION('center_axis',(0.,1.,0.));
#12061=DIRECTION('ref_axis',(1.,0.,0.));
#12062=DIRECTION('',(0.,1.,0.));
#12063=DIRECTION('center_axis',(0.,-1.,0.));
#12064=DIRECTION('ref_axis',(1.,0.,0.));
#12065=DIRECTION('center_axis',(0.,1.,0.));
#12066=DIRECTION('ref_axis',(0.565264218607056,0.,-0.824909912149536));
#12067=DIRECTION('',(0.,-1.,0.));
#12068=DIRECTION('center_axis',(0.,1.,0.));
#12069=DIRECTION('ref_axis',(1.,0.,0.));
#12070=DIRECTION('',(0.,1.,0.));
#12071=DIRECTION('center_axis',(0.,1.,0.));
#12072=DIRECTION('ref_axis',(1.,0.,0.));
#12073=DIRECTION('center_axis',(-0.824909912149536,0.,-0.565264218607055));
#12074=DIRECTION('ref_axis',(-0.565264218607055,0.,0.824909912149537));
#12075=DIRECTION('',(-0.565264218607055,0.,0.824909912149537));
#12076=DIRECTION('',(0.,-1.,0.));
#12077=DIRECTION('',(-0.565264218607055,0.,0.824909912149537));
#12078=DIRECTION('center_axis',(0.,1.,0.));
#12079=DIRECTION('ref_axis',(1.,0.,0.));
#12080=DIRECTION('',(0.565264218607055,0.,-0.824909912149537));
#12081=DIRECTION('center_axis',(0.,1.,0.));
#12082=DIRECTION('ref_axis',(1.,0.,0.));
#12083=DIRECTION('center_axis',(0.824909912149536,0.,0.565264218607055));
#12084=DIRECTION('ref_axis',(0.565264218607055,0.,-0.824909912149537));
#12085=DIRECTION('',(0.565264218607055,0.,-0.824909912149537));
#12086=DIRECTION('',(0.,1.,0.));
#12087=DIRECTION('center_axis',(0.,1.,0.));
#12088=DIRECTION('ref_axis',(-0.565264218607055,0.,0.824909912149536));
#12089=DIRECTION('center_axis',(0.,1.,0.));
#12090=DIRECTION('ref_axis',(1.,0.,0.));
#12091=DIRECTION('center_axis',(0.,1.,0.));
#12092=DIRECTION('ref_axis',(1.,0.,0.));
#12093=DIRECTION('axis',(0.,0.,1.));
#12094=DIRECTION('refdir',(1.,0.,0.));
#12095=DIRECTION('center_axis',(0.,1.,0.));
#12096=DIRECTION('ref_axis',(1.,0.,0.));
#12097=DIRECTION('center_axis',(0.,-1.,0.));
#12098=DIRECTION('ref_axis',(1.,0.,0.));
#12099=DIRECTION('',(0.,-1.,0.));
#12100=DIRECTION('center_axis',(0.,-1.,0.));
#12101=DIRECTION('ref_axis',(1.,0.,0.));
#12102=DIRECTION('center_axis',(0.,1.,0.));
#12103=DIRECTION('ref_axis',(1.,0.,0.));
#12104=DIRECTION('center_axis',(0.,1.,0.));
#12105=DIRECTION('ref_axis',(1.,0.,0.));
#12106=DIRECTION('',(0.,-1.,0.));
#12107=DIRECTION('center_axis',(0.,1.,0.));
#12108=DIRECTION('ref_axis',(1.,0.,0.));
#12109=DIRECTION('center_axis',(0.,1.,0.));
#12110=DIRECTION('ref_axis',(1.,0.,0.));
#12111=DIRECTION('center_axis',(0.,1.,0.));
#12112=DIRECTION('ref_axis',(1.,0.,0.));
#12113=DIRECTION('axis',(0.,0.,1.));
#12114=DIRECTION('refdir',(1.,0.,0.));
#12115=DIRECTION('center_axis',(0.,1.,0.));
#12116=DIRECTION('ref_axis',(1.,0.,0.));
#12117=DIRECTION('center_axis',(0.,-1.,0.));
#12118=DIRECTION('ref_axis',(1.,0.,0.));
#12119=DIRECTION('',(0.,-1.,0.));
#12120=DIRECTION('center_axis',(0.,-1.,0.));
#12121=DIRECTION('ref_axis',(1.,0.,0.));
#12122=DIRECTION('center_axis',(0.,1.,0.));
#12123=DIRECTION('ref_axis',(1.,0.,0.));
#12124=DIRECTION('center_axis',(0.,1.,0.));
#12125=DIRECTION('ref_axis',(1.,0.,0.));
#12126=DIRECTION('',(0.,-1.,0.));
#12127=DIRECTION('center_axis',(0.,1.,0.));
#12128=DIRECTION('ref_axis',(1.,0.,0.));
#12129=DIRECTION('center_axis',(0.,1.,0.));
#12130=DIRECTION('ref_axis',(1.,0.,0.));
#12131=DIRECTION('center_axis',(0.,1.,0.));
#12132=DIRECTION('ref_axis',(1.,0.,0.));
#12133=DIRECTION('',(0.,0.,1.));
#12134=DIRECTION('',(1.,0.,0.));
#12135=DIRECTION('',(0.,0.,1.));
#12136=DIRECTION('',(1.,0.,0.));
#12137=DIRECTION('',(0.,0.,1.));
#12138=DIRECTION('',(1.,0.,0.));
#12139=DIRECTION('axis',(0.,0.,1.));
#12140=DIRECTION('refdir',(1.,0.,0.));
#12141=DIRECTION('axis',(0.,0.,1.));
#12142=DIRECTION('refdir',(1.,0.,0.));
#12143=DIRECTION('center_axis',(0.,1.,0.));
#12144=DIRECTION('ref_axis',(1.,0.,0.));
#12145=DIRECTION('center_axis',(0.,1.,0.));
#12146=DIRECTION('ref_axis',(1.,0.,0.));
#12147=DIRECTION('',(0.,1.,0.));
#12148=DIRECTION('center_axis',(0.,1.,0.));
#12149=DIRECTION('ref_axis',(1.,0.,0.));
#12150=DIRECTION('center_axis',(0.,1.,0.));
#12151=DIRECTION('ref_axis',(1.,0.,0.));
#12152=DIRECTION('center_axis',(0.,1.,0.));
#12153=DIRECTION('ref_axis',(0.,0.,1.));
#12154=DIRECTION('',(0.,0.,1.));
#12155=DIRECTION('',(-1.,0.,0.));
#12156=DIRECTION('',(0.,0.,-1.));
#12157=DIRECTION('',(1.,0.,0.));
#12158=DIRECTION('center_axis',(1.,0.,0.));
#12159=DIRECTION('ref_axis',(0.,1.,0.));
#12160=DIRECTION('',(0.,1.,0.));
#12161=DIRECTION('',(0.,0.,-1.));
#12162=DIRECTION('',(0.,-1.,0.));
#12163=DIRECTION('',(0.,0.,1.));
#12164=DIRECTION('',(0.,1.,0.));
#12165=DIRECTION('center_axis',(0.,0.,1.));
#12166=DIRECTION('ref_axis',(1.,0.,0.));
#12167=DIRECTION('',(0.,-1.,0.));
#12168=DIRECTION('center_axis',(0.,0.,-1.));
#12169=DIRECTION('ref_axis',(1.,0.,0.));
#12170=DIRECTION('center_axis',(-1.,0.,0.));
#12171=DIRECTION('ref_axis',(0.,-1.,0.));
#12172=DIRECTION('',(0.,-1.,0.));
#12173=DIRECTION('',(0.,0.,1.));
#12174=DIRECTION('',(0.,1.,0.));
#12175=DIRECTION('',(0.,0.,1.));
#12176=DIRECTION('center_axis',(0.,1.,0.));
#12177=DIRECTION('ref_axis',(-1.,0.,0.));
#12178=DIRECTION('',(0.,0.,-1.));
#12179=DIRECTION('',(-1.,0.,0.));
#12180=DIRECTION('',(1.,0.,0.));
#12181=DIRECTION('center_axis',(0.,1.,0.));
#12182=DIRECTION('ref_axis',(-1.,0.,0.));
#12183=DIRECTION('',(1.,0.,0.));
#12184=DIRECTION('',(-1.,0.,0.));
#12185=DIRECTION('',(0.,0.,1.));
#12186=DIRECTION('center_axis',(0.,0.,1.));
#12187=DIRECTION('ref_axis',(1.,0.,0.));
#12188=DIRECTION('center_axis',(0.,0.,1.));
#12189=DIRECTION('ref_axis',(1.,0.,0.));
#12190=DIRECTION('center_axis',(0.,0.,1.));
#12191=DIRECTION('ref_axis',(1.,0.,0.));
#12192=DIRECTION('center_axis',(0.,0.,1.));
#12193=DIRECTION('ref_axis',(1.,0.,0.));
#12194=DIRECTION('',(0.,0.,-1.));
#12195=DIRECTION('center_axis',(0.,0.,1.));
#12196=DIRECTION('ref_axis',(1.,0.,0.));
#12197=DIRECTION('center_axis',(0.,0.,1.));
#12198=DIRECTION('ref_axis',(1.,0.,0.));
#12199=DIRECTION('center_axis',(0.,0.,1.));
#12200=DIRECTION('ref_axis',(1.,0.,0.));
#12201=DIRECTION('center_axis',(0.,0.,1.));
#12202=DIRECTION('ref_axis',(1.,0.,0.));
#12203=DIRECTION('center_axis',(0.,0.,1.));
#12204=DIRECTION('ref_axis',(1.,0.,0.));
#12205=DIRECTION('',(0.,0.,-1.));
#12206=DIRECTION('center_axis',(0.,0.,1.));
#12207=DIRECTION('ref_axis',(1.,0.,0.));
#12208=DIRECTION('center_axis',(0.,0.,1.));
#12209=DIRECTION('ref_axis',(1.,0.,0.));
#12210=DIRECTION('center_axis',(0.,0.,1.));
#12211=DIRECTION('ref_axis',(1.,0.,0.));
#12212=DIRECTION('center_axis',(1.,0.,0.));
#12213=DIRECTION('ref_axis',(0.,0.,-1.));
#12214=DIRECTION('',(0.,1.,0.));
#12215=DIRECTION('center_axis',(1.,0.,0.));
#12216=DIRECTION('ref_axis',(0.,0.,-1.));
#12217=DIRECTION('center_axis',(1.,0.,0.));
#12218=DIRECTION('ref_axis',(0.,0.,-1.));
#12219=DIRECTION('center_axis',(1.,0.,0.));
#12220=DIRECTION('ref_axis',(0.,0.,-1.));
#12221=DIRECTION('',(1.,0.,0.));
#12222=DIRECTION('center_axis',(-1.,0.,0.));
#12223=DIRECTION('ref_axis',(0.,0.,-1.));
#12224=DIRECTION('center_axis',(1.,0.,0.));
#12225=DIRECTION('ref_axis',(0.,0.,-1.));
#12226=DIRECTION('center_axis',(1.,0.,0.));
#12227=DIRECTION('ref_axis',(0.,0.,-1.));
#12228=DIRECTION('',(0.,-1.,0.));
#12229=DIRECTION('center_axis',(0.,1.,0.));
#12230=DIRECTION('ref_axis',(1.,0.,0.));
#12231=DIRECTION('center_axis',(0.,1.,0.));
#12232=DIRECTION('ref_axis',(1.,0.,0.));
#12233=DIRECTION('',(0.,1.,0.));
#12234=DIRECTION('center_axis',(0.,-1.,0.));
#12235=DIRECTION('ref_axis',(1.,0.,0.));
#12236=DIRECTION('center_axis',(0.,-1.,0.));
#12237=DIRECTION('ref_axis',(1.,0.,0.));
#12238=DIRECTION('',(1.,0.,0.));
#12239=DIRECTION('',(0.,0.,1.));
#12240=DIRECTION('',(1.,0.,0.));
#12241=DIRECTION('',(0.,0.,1.));
#12242=DIRECTION('center_axis',(-1.,0.,0.));
#12243=DIRECTION('ref_axis',(0.,-1.,0.));
#12244=DIRECTION('',(0.,0.,-1.));
#12245=DIRECTION('',(0.,-1.,0.));
#12246=DIRECTION('',(0.,-1.,0.));
#12247=DIRECTION('center_axis',(0.,0.,1.));
#12248=DIRECTION('ref_axis',(1.,0.,0.));
#12249=DIRECTION('',(-1.,0.,0.));
#12250=DIRECTION('',(0.,1.,0.));
#12251=DIRECTION('center_axis',(0.,0.,1.));
#12252=DIRECTION('ref_axis',(1.,0.,0.));
#12253=DIRECTION('',(1.,0.,0.));
#12254=DIRECTION('',(0.,1.,0.));
#12255=DIRECTION('center_axis',(1.,0.,0.));
#12256=DIRECTION('ref_axis',(0.,1.,0.));
#12257=DIRECTION('',(0.,0.,1.));
#12258=DIRECTION('center_axis',(0.,1.,0.));
#12259=DIRECTION('ref_axis',(1.,0.,0.));
#12260=DIRECTION('axis',(0.,0.,1.));
#12261=DIRECTION('refdir',(1.,0.,0.));
#12262=DIRECTION('center_axis',(0.,1.,0.));
#12263=DIRECTION('ref_axis',(1.,0.,0.));
#12264=DIRECTION('center_axis',(0.,1.,0.));
#12265=DIRECTION('ref_axis',(1.,0.,0.));
#12266=DIRECTION('center_axis',(0.,1.,0.));
#12267=DIRECTION('ref_axis',(1.,0.,0.));
#12268=DIRECTION('center_axis',(0.,1.,0.));
#12269=DIRECTION('ref_axis',(1.,0.,0.));
#12270=DIRECTION('',(0.,-1.,0.));
#12271=DIRECTION('center_axis',(0.,1.,0.));
#12272=DIRECTION('ref_axis',(1.,0.,0.));
#12273=DIRECTION('center_axis',(0.,1.,0.));
#12274=DIRECTION('ref_axis',(1.,0.,0.));
#12275=DIRECTION('center_axis',(0.,1.,0.));
#12276=DIRECTION('ref_axis',(1.,0.,0.));
#12277=DIRECTION('center_axis',(0.,1.,0.));
#12278=DIRECTION('ref_axis',(1.,0.,0.));
#12279=DIRECTION('',(0.,-1.,0.));
#12280=DIRECTION('center_axis',(0.,1.,0.));
#12281=DIRECTION('ref_axis',(1.,0.,0.));
#12282=DIRECTION('axis',(0.,0.,1.));
#12283=DIRECTION('refdir',(1.,0.,0.));
#12284=DIRECTION('center_axis',(0.,0.,1.));
#12285=DIRECTION('ref_axis',(1.,0.,0.));
#12286=DIRECTION('center_axis',(0.,0.,1.));
#12287=DIRECTION('ref_axis',(1.,0.,0.));
#12288=DIRECTION('',(0.,0.,-1.));
#12289=DIRECTION('center_axis',(0.,0.,1.));
#12290=DIRECTION('ref_axis',(1.,0.,0.));
#12291=DIRECTION('center_axis',(0.,0.,1.));
#12292=DIRECTION('ref_axis',(1.,0.,0.));
#12293=DIRECTION('center_axis',(0.,0.,1.));
#12294=DIRECTION('ref_axis',(1.,0.,0.));
#12295=DIRECTION('axis',(0.,0.,1.));
#12296=DIRECTION('refdir',(1.,0.,0.));
#12297=DIRECTION('center_axis',(0.866025403784439,0.,-0.5));
#12298=DIRECTION('ref_axis',(0.5,0.,0.866025403784439));
#12299=DIRECTION('',(0.5,0.,0.866025403784439));
#12300=DIRECTION('',(0.,-1.,0.));
#12301=DIRECTION('',(0.5,0.,0.866025403784439));
#12302=DIRECTION('',(0.,-1.,0.));
#12303=DIRECTION('center_axis',(1.20185167898973E-16,0.,-1.));
#12304=DIRECTION('ref_axis',(1.,0.,1.20185167898973E-16));
#12305=DIRECTION('',(1.,0.,1.20185167898973E-16));
#12306=DIRECTION('',(0.,-1.,0.));
#12307=DIRECTION('',(1.,0.,1.20185167898973E-16));
#12308=DIRECTION('center_axis',(-0.866025403784439,0.,-0.5));
#12309=DIRECTION('ref_axis',(0.5,0.,-0.866025403784439));
#12310=DIRECTION('',(0.5,0.,-0.866025403784439));
#12311=DIRECTION('',(0.,-1.,0.));
#12312=DIRECTION('',(0.5,0.,-0.866025403784439));
#12313=DIRECTION('center_axis',(-0.866025403784439,0.,0.5));
#12314=DIRECTION('ref_axis',(-0.5,0.,-0.866025403784439));
#12315=DIRECTION('',(-0.5,0.,-0.866025403784439));
#12316=DIRECTION('',(0.,-1.,0.));
#12317=DIRECTION('',(-0.5,0.,-0.866025403784439));
#12318=DIRECTION('center_axis',(-2.40370335797945E-16,0.,1.));
#12319=DIRECTION('ref_axis',(-1.,0.,-2.40370335797945E-16));
#12320=DIRECTION('',(-1.,0.,-2.40370335797945E-16));
#12321=DIRECTION('',(0.,-1.,0.));
#12322=DIRECTION('',(-1.,0.,-2.40370335797945E-16));
#12323=DIRECTION('center_axis',(0.866025403784439,0.,0.5));
#12324=DIRECTION('ref_axis',(-0.5,0.,0.866025403784439));
#12325=DIRECTION('',(-0.5,0.,0.866025403784439));
#12326=DIRECTION('',(-0.5,0.,0.866025403784439));
#12327=DIRECTION('center_axis',(0.,-1.,0.));
#12328=DIRECTION('ref_axis',(0.,0.,-1.));
#12329=DIRECTION('center_axis',(0.,1.,0.));
#12330=DIRECTION('ref_axis',(0.,0.,1.));
#12331=DIRECTION('center_axis',(0.,-1.,0.));
#12332=DIRECTION('ref_axis',(1.,0.,0.));
#12333=DIRECTION('center_axis',(0.,-1.,0.));
#12334=DIRECTION('ref_axis',(1.,0.,0.));
#12335=DIRECTION('center_axis',(0.,-1.,0.));
#12336=DIRECTION('ref_axis',(1.,0.,0.));
#12337=DIRECTION('',(0.707106781186548,0.707106781186547,8.65956056235494E-17));
#12338=DIRECTION('center_axis',(0.,-1.,0.));
#12339=DIRECTION('ref_axis',(1.,0.,0.));
#12340=DIRECTION('center_axis',(0.,1.,0.));
#12341=DIRECTION('ref_axis',(1.,0.,0.));
#12342=DIRECTION('',(0.,1.,0.));
#12343=DIRECTION('center_axis',(0.,1.,0.));
#12344=DIRECTION('ref_axis',(1.,0.,0.));
#12345=DIRECTION('center_axis',(0.,-1.,0.));
#12346=DIRECTION('ref_axis',(1.,0.,0.));
#12347=DIRECTION('',(-0.707106781186548,0.707106781186547,-8.65956056235494E-17));
#12348=DIRECTION('center_axis',(0.,-1.,0.));
#12349=DIRECTION('ref_axis',(0.,0.,-1.));
#12350=DIRECTION('',(0.,0.,1.));
#12351=DIRECTION('',(1.,0.,0.));
#12352=DIRECTION('',(0.,0.,1.));
#12353=DIRECTION('',(1.,0.,0.));
#12354=DIRECTION('',(0.,0.,1.));
#12355=DIRECTION('',(1.,0.,0.));
#12356=DIRECTION('',(0.,0.,1.));
#12357=DIRECTION('',(2.22044604925031E-16,-1.,0.));
#12358=DIRECTION('',(0.,0.,1.));
#12359=DIRECTION('',(1.,0.,0.));
#12360=DIRECTION('',(0.,0.,1.));
#12361=DIRECTION('',(1.,0.,0.));
#12362=DIRECTION('',(0.,0.,1.));
#12363=DIRECTION('',(1.,0.,0.));
#12364=DIRECTION('',(0.,0.,1.));
#12365=DIRECTION('',(1.,0.,0.));
#12366=CARTESIAN_POINT('',(0.,0.,0.));
#12367=CARTESIAN_POINT('',(0.,0.,0.));
#12368=CARTESIAN_POINT('',(0.,0.,0.));
#12369=CARTESIAN_POINT('Origin',(1.5,-4.5,-0.1));
#12370=CARTESIAN_POINT('',(1.275,-4.5,0.));
#12371=CARTESIAN_POINT('Origin',(1.5,-4.5,0.));
#12372=CARTESIAN_POINT('',(1.275,-4.5,1.));
#12373=CARTESIAN_POINT('',(1.275,-4.5,-0.1));
#12374=CARTESIAN_POINT('Origin',(1.5,-4.5,1.));
#12375=CARTESIAN_POINT('Origin',(1.5,2.,-0.1));
#12376=CARTESIAN_POINT('',(1.275,2.,0.));
#12377=CARTESIAN_POINT('Origin',(1.5,2.,0.));
#12378=CARTESIAN_POINT('',(1.275,2.,1.));
#12379=CARTESIAN_POINT('',(1.275,2.,-0.1));
#12380=CARTESIAN_POINT('Origin',(1.5,2.,1.));
#12381=CARTESIAN_POINT('Origin',(-1.5,-4.5,-0.1));
#12382=CARTESIAN_POINT('',(-1.725,-4.5,0.));
#12383=CARTESIAN_POINT('Origin',(-1.5,-4.5,0.));
#12384=CARTESIAN_POINT('',(-1.725,-4.5,1.));
#12385=CARTESIAN_POINT('',(-1.725,-4.5,-0.1));
#12386=CARTESIAN_POINT('Origin',(-1.5,-4.5,1.));
#12387=CARTESIAN_POINT('Origin',(-1.5,2.,-0.1));
#12388=CARTESIAN_POINT('',(-1.725,2.,0.));
#12389=CARTESIAN_POINT('Origin',(-1.5,2.,0.));
#12390=CARTESIAN_POINT('',(-1.725,2.,1.));
#12391=CARTESIAN_POINT('',(-1.725,2.,-0.1));
#12392=CARTESIAN_POINT('Origin',(-1.5,2.,1.));
#12393=CARTESIAN_POINT('Origin',(-6.,-1.4,-0.1));
#12394=CARTESIAN_POINT('',(-6.21,-1.4,0.));
#12395=CARTESIAN_POINT('Origin',(-6.,-1.4,0.));
#12396=CARTESIAN_POINT('',(-6.21,-1.4,1.));
#12397=CARTESIAN_POINT('',(-6.21,-1.4,-0.1));
#12398=CARTESIAN_POINT('Origin',(-6.,-1.4,1.));
#12399=CARTESIAN_POINT('Origin',(-8.5,1.4,-0.1));
#12400=CARTESIAN_POINT('',(-8.71,1.4,0.));
#12401=CARTESIAN_POINT('Origin',(-8.5,1.4,0.));
#12402=CARTESIAN_POINT('',(-8.71,1.4,1.));
#12403=CARTESIAN_POINT('',(-8.71,1.4,-0.1));
#12404=CARTESIAN_POINT('Origin',(-8.5,1.4,1.));
#12405=CARTESIAN_POINT('Origin',(-8.5,-1.4,-0.1));
#12406=CARTESIAN_POINT('',(-8.71,-1.4,0.));
#12407=CARTESIAN_POINT('Origin',(-8.5,-1.4,0.));
#12408=CARTESIAN_POINT('',(-8.71,-1.4,1.));
#12409=CARTESIAN_POINT('',(-8.71,-1.4,-0.1));
#12410=CARTESIAN_POINT('Origin',(-8.5,-1.4,1.));
#12411=CARTESIAN_POINT('Origin',(-6.,1.4,-0.1));
#12412=CARTESIAN_POINT('',(-6.21,1.4,0.));
#12413=CARTESIAN_POINT('Origin',(-6.,1.4,0.));
#12414=CARTESIAN_POINT('',(-6.21,1.4,1.));
#12415=CARTESIAN_POINT('',(-6.21,1.4,-0.1));
#12416=CARTESIAN_POINT('Origin',(-6.,1.4,1.));
#12417=CARTESIAN_POINT('Origin',(2.5,4.,-0.1));
#12418=CARTESIAN_POINT('',(2.225,4.,0.));
#12419=CARTESIAN_POINT('Origin',(2.5,4.,0.));
#12420=CARTESIAN_POINT('',(2.225,4.,1.));
#12421=CARTESIAN_POINT('',(2.225,4.,-0.1));
#12422=CARTESIAN_POINT('Origin',(2.5,4.,1.));
#12423=CARTESIAN_POINT('Origin',(-4.5,4.,-0.1));
#12424=CARTESIAN_POINT('',(-4.775,4.,0.));
#12425=CARTESIAN_POINT('Origin',(-4.5,4.,0.));
#12426=CARTESIAN_POINT('',(-4.775,4.,1.));
#12427=CARTESIAN_POINT('',(-4.775,4.,-0.1));
#12428=CARTESIAN_POINT('Origin',(-4.5,4.,1.));
#12429=CARTESIAN_POINT('Origin',(2.5,-6.,-0.1));
#12430=CARTESIAN_POINT('',(2.225,-6.,0.));
#12431=CARTESIAN_POINT('Origin',(2.5,-6.,0.));
#12432=CARTESIAN_POINT('',(2.225,-6.,1.));
#12433=CARTESIAN_POINT('',(2.225,-6.,-0.1));
#12434=CARTESIAN_POINT('Origin',(2.5,-6.,1.));
#12435=CARTESIAN_POINT('Origin',(-4.5,-6.,-0.1));
#12436=CARTESIAN_POINT('',(-4.775,-6.,0.));
#12437=CARTESIAN_POINT('Origin',(-4.5,-6.,0.));
#12438=CARTESIAN_POINT('',(-4.775,-6.,1.));
#12439=CARTESIAN_POINT('',(-4.775,-6.,-0.1));
#12440=CARTESIAN_POINT('Origin',(-4.5,-6.,1.));
#12441=CARTESIAN_POINT('Origin',(3.5,4.5,0.));
#12442=CARTESIAN_POINT('',(3.5,4.5,0.));
#12443=CARTESIAN_POINT('',(-9.5,4.5,0.));
#12444=CARTESIAN_POINT('',(3.5,4.5,0.));
#12445=CARTESIAN_POINT('',(-9.5,4.5,1.));
#12446=CARTESIAN_POINT('',(-9.5,4.5,0.));
#12447=CARTESIAN_POINT('',(3.5,4.5,1.));
#12448=CARTESIAN_POINT('',(3.5,4.5,1.));
#12449=CARTESIAN_POINT('',(3.5,4.5,0.));
#12450=CARTESIAN_POINT('Origin',(3.5,-7.,0.));
#12451=CARTESIAN_POINT('',(3.5,-7.,0.));
#12452=CARTESIAN_POINT('',(3.5,-7.,0.));
#12453=CARTESIAN_POINT('',(3.5,-7.,1.));
#12454=CARTESIAN_POINT('',(3.5,-7.,1.));
#12455=CARTESIAN_POINT('',(3.5,-7.,0.));
#12456=CARTESIAN_POINT('Origin',(-9.5,-7.,0.));
#12457=CARTESIAN_POINT('',(-9.5,-7.,0.));
#12458=CARTESIAN_POINT('',(-9.5,-7.,0.));
#12459=CARTESIAN_POINT('',(-9.5,-7.,1.));
#12460=CARTESIAN_POINT('',(-9.5,-7.,1.));
#12461=CARTESIAN_POINT('',(-9.5,-7.,0.));
#12462=CARTESIAN_POINT('Origin',(-9.5,4.5,0.));
#12463=CARTESIAN_POINT('',(-9.5,4.5,0.));
#12464=CARTESIAN_POINT('',(-9.5,4.5,1.));
#12465=CARTESIAN_POINT('Origin',(-3.,-1.25,1.));
#12466=CARTESIAN_POINT('Origin',(-3.,-1.25,0.));
#12467=CARTESIAN_POINT('',(0.,0.,0.));
#12468=CARTESIAN_POINT('Origin',(2.5,4.,-2.9));
#12469=CARTESIAN_POINT('',(2.225,4.,-2.8));
#12470=CARTESIAN_POINT('Origin',(2.5,4.,-2.8));
#12471=CARTESIAN_POINT('',(2.225,4.,-2.));
#12472=CARTESIAN_POINT('',(2.225,4.,-2.9));
#12473=CARTESIAN_POINT('Origin',(2.5,4.,-2.));
#12474=CARTESIAN_POINT('Origin',(-4.5,4.,-2.9));
#12475=CARTESIAN_POINT('',(-4.775,4.,-2.8));
#12476=CARTESIAN_POINT('Origin',(-4.5,4.,-2.8));
#12477=CARTESIAN_POINT('',(-4.775,4.,-2.));
#12478=CARTESIAN_POINT('',(-4.775,4.,-2.9));
#12479=CARTESIAN_POINT('Origin',(-4.5,4.,-2.));
#12480=CARTESIAN_POINT('Origin',(2.5,-6.,-2.9));
#12481=CARTESIAN_POINT('',(2.225,-6.,-2.8));
#12482=CARTESIAN_POINT('Origin',(2.5,-6.,-2.8));
#12483=CARTESIAN_POINT('',(2.225,-6.,-2.));
#12484=CARTESIAN_POINT('',(2.225,-6.,-2.9));
#12485=CARTESIAN_POINT('Origin',(2.5,-6.,-2.));
#12486=CARTESIAN_POINT('Origin',(-4.5,-6.,-2.9));
#12487=CARTESIAN_POINT('',(-4.775,-6.,-2.8));
#12488=CARTESIAN_POINT('Origin',(-4.5,-6.,-2.8));
#12489=CARTESIAN_POINT('',(-4.775,-6.,-2.));
#12490=CARTESIAN_POINT('',(-4.775,-6.,-2.9));
#12491=CARTESIAN_POINT('Origin',(-4.5,-6.,-2.));
#12492=CARTESIAN_POINT('Origin',(10.5,4.5,-2.8));
#12493=CARTESIAN_POINT('',(10.5,4.5,-2.8));
#12494=CARTESIAN_POINT('',(-9.5,4.5,-2.8));
#12495=CARTESIAN_POINT('',(10.5,4.5,-2.8));
#12496=CARTESIAN_POINT('',(-9.5,4.5,-2.));
#12497=CARTESIAN_POINT('',(-9.5,4.5,-2.8));
#12498=CARTESIAN_POINT('',(10.5,4.5,-2.));
#12499=CARTESIAN_POINT('',(10.5,4.5,-2.));
#12500=CARTESIAN_POINT('',(10.5,4.5,-2.8));
#12501=CARTESIAN_POINT('Origin',(10.5,-7.,-2.8));
#12502=CARTESIAN_POINT('',(10.5,-7.,-2.8));
#12503=CARTESIAN_POINT('',(10.5,-7.,-2.8));
#12504=CARTESIAN_POINT('',(10.5,-7.,-2.));
#12505=CARTESIAN_POINT('',(10.5,-7.,-2.));
#12506=CARTESIAN_POINT('',(10.5,-7.,-2.8));
#12507=CARTESIAN_POINT('Origin',(-9.5,-7.,-2.8));
#12508=CARTESIAN_POINT('',(-9.5,-7.,-2.8));
#12509=CARTESIAN_POINT('',(-9.5,-7.,-2.8));
#12510=CARTESIAN_POINT('',(-9.5,-7.,-2.));
#12511=CARTESIAN_POINT('',(-9.5,-7.,-2.));
#12512=CARTESIAN_POINT('',(-9.5,-7.,-2.8));
#12513=CARTESIAN_POINT('Origin',(-9.5,4.5,-2.8));
#12514=CARTESIAN_POINT('',(-9.5,4.5,-2.8));
#12515=CARTESIAN_POINT('',(-9.5,4.5,-2.));
#12516=CARTESIAN_POINT('Origin',(0.5,-1.25,-2.));
#12517=CARTESIAN_POINT('Origin',(0.5,-1.25,-2.8));
#12518=CARTESIAN_POINT('',(0.,0.,0.));
#12519=CARTESIAN_POINT('Origin',(-8.5,4.5,-3.6));
#12520=CARTESIAN_POINT('',(-8.5,4.5,-3.6));
#12521=CARTESIAN_POINT('',(-9.5,4.5,-3.6));
#12522=CARTESIAN_POINT('',(-8.5,4.5,-3.6));
#12523=CARTESIAN_POINT('',(-9.5,4.5,-2.8));
#12524=CARTESIAN_POINT('',(-9.5,4.5,-3.6));
#12525=CARTESIAN_POINT('',(-8.5,4.5,-2.8));
#12526=CARTESIAN_POINT('',(-8.5,4.5,-2.8));
#12527=CARTESIAN_POINT('',(-8.5,4.5,-3.6));
#12528=CARTESIAN_POINT('Origin',(-8.5,-7.,-3.6));
#12529=CARTESIAN_POINT('',(-8.5,-7.,-3.6));
#12530=CARTESIAN_POINT('',(-8.5,-7.,-3.6));
#12531=CARTESIAN_POINT('',(-8.5,-7.,-2.8));
#12532=CARTESIAN_POINT('',(-8.5,-7.,-2.8));
#12533=CARTESIAN_POINT('',(-8.5,-7.,-3.6));
#12534=CARTESIAN_POINT('Origin',(-9.5,-7.,-3.6));
#12535=CARTESIAN_POINT('',(-9.5,-7.,-3.6));
#12536=CARTESIAN_POINT('',(-9.5,-7.,-3.6));
#12537=CARTESIAN_POINT('',(-9.5,-7.,-2.8));
#12538=CARTESIAN_POINT('',(-9.5,-7.,-2.8));
#12539=CARTESIAN_POINT('',(-9.5,-7.,-3.6));
#12540=CARTESIAN_POINT('Origin',(-9.5,4.5,-3.6));
#12541=CARTESIAN_POINT('',(-9.5,4.5,-3.6));
#12542=CARTESIAN_POINT('',(-9.5,4.5,-2.8));
#12543=CARTESIAN_POINT('Origin',(-9.,-1.25,-2.8));
#12544=CARTESIAN_POINT('Origin',(-9.,-1.25,-3.6));
#12545=CARTESIAN_POINT('',(0.,0.,0.));
#12546=CARTESIAN_POINT('Origin',(10.5,4.5,-3.6));
#12547=CARTESIAN_POINT('',(10.5,4.5,-3.6));
#12548=CARTESIAN_POINT('',(9.5,4.5,-3.6));
#12549=CARTESIAN_POINT('',(10.5,4.5,-3.6));
#12550=CARTESIAN_POINT('',(9.5,4.5,-2.8));
#12551=CARTESIAN_POINT('',(9.5,4.5,-3.6));
#12552=CARTESIAN_POINT('',(10.5,4.5,-2.8));
#12553=CARTESIAN_POINT('',(10.5,4.5,-2.8));
#12554=CARTESIAN_POINT('',(10.5,4.5,-3.6));
#12555=CARTESIAN_POINT('Origin',(10.5,-7.,-3.6));
#12556=CARTESIAN_POINT('',(10.5,-7.,-3.6));
#12557=CARTESIAN_POINT('',(10.5,-7.,-3.6));
#12558=CARTESIAN_POINT('',(10.5,-7.,-2.8));
#12559=CARTESIAN_POINT('',(10.5,-7.,-2.8));
#12560=CARTESIAN_POINT('',(10.5,-7.,-3.6));
#12561=CARTESIAN_POINT('Origin',(9.5,-7.,-3.6));
#12562=CARTESIAN_POINT('',(9.5,-7.,-3.6));
#12563=CARTESIAN_POINT('',(9.5,-7.,-3.6));
#12564=CARTESIAN_POINT('',(9.5,-7.,-2.8));
#12565=CARTESIAN_POINT('',(9.5,-7.,-2.8));
#12566=CARTESIAN_POINT('',(9.5,-7.,-3.6));
#12567=CARTESIAN_POINT('Origin',(9.5,4.5,-3.6));
#12568=CARTESIAN_POINT('',(9.5,4.5,-3.6));
#12569=CARTESIAN_POINT('',(9.5,4.5,-2.8));
#12570=CARTESIAN_POINT('Origin',(10.,-1.25,-2.8));
#12571=CARTESIAN_POINT('Origin',(10.,-1.25,-3.6));
#12572=CARTESIAN_POINT('',(0.,0.,0.));
#12573=CARTESIAN_POINT('Origin',(-5.25982293614231,-0.9,14.8604204653858));
#12574=CARTESIAN_POINT('',(-5.48482293614231,-0.8,14.8604204653858));
#12575=CARTESIAN_POINT('Origin',(-5.25982293614231,-0.8,14.8604204653858));
#12576=CARTESIAN_POINT('',(-5.48482293614231,0.8,14.8604204653858));
#12577=CARTESIAN_POINT('',(-5.48482293614231,-0.9,14.8604204653858));
#12578=CARTESIAN_POINT('Origin',(-5.25982293614231,0.8,14.8604204653858));
#12579=CARTESIAN_POINT('Origin',(-1.13137084989848,-1.13137084989848,15.8));
#12580=CARTESIAN_POINT('',(-1.29637084989848,-1.13137084989848,15.8));
#12581=CARTESIAN_POINT('Origin',(-1.13137084989848,-1.13137084989848,15.8));
#12582=CARTESIAN_POINT('',(-1.29637084989848,-1.13137084989848,16.5));
#12583=CARTESIAN_POINT('',(-1.29637084989848,-1.13137084989848,15.8));
#12584=CARTESIAN_POINT('Origin',(-1.13137084989848,-1.13137084989848,16.5));
#12585=CARTESIAN_POINT('Origin',(-1.13137084989848,-1.13137084989848,15.8));
#12586=CARTESIAN_POINT('Origin',(-1.13137084989848,1.13137084989848,15.8));
#12587=CARTESIAN_POINT('',(-1.29637084989848,1.13137084989848,15.8));
#12588=CARTESIAN_POINT('Origin',(-1.13137084989848,1.13137084989848,15.8));
#12589=CARTESIAN_POINT('',(-1.29637084989848,1.13137084989848,16.5));
#12590=CARTESIAN_POINT('',(-1.29637084989848,1.13137084989848,15.8));
#12591=CARTESIAN_POINT('Origin',(-1.13137084989848,1.13137084989848,16.5));
#12592=CARTESIAN_POINT('Origin',(-1.13137084989848,1.13137084989848,15.8));
#12593=CARTESIAN_POINT('Origin',(1.13137084989848,1.13137084989848,15.8));
#12594=CARTESIAN_POINT('',(0.966370849898476,1.13137084989848,15.8));
#12595=CARTESIAN_POINT('Origin',(1.13137084989848,1.13137084989848,15.8));
#12596=CARTESIAN_POINT('',(0.966370849898476,1.13137084989848,16.5));
#12597=CARTESIAN_POINT('',(0.966370849898476,1.13137084989848,15.8));
#12598=CARTESIAN_POINT('Origin',(1.13137084989848,1.13137084989848,16.5));
#12599=CARTESIAN_POINT('Origin',(1.13137084989848,1.13137084989848,15.8));
#12600=CARTESIAN_POINT('Origin',(1.13137084989848,-1.13137084989848,15.8));
#12601=CARTESIAN_POINT('',(0.966370849898476,-1.13137084989848,15.8));
#12602=CARTESIAN_POINT('Origin',(1.13137084989848,-1.13137084989848,15.8));
#12603=CARTESIAN_POINT('',(0.966370849898476,-1.13137084989848,16.5));
#12604=CARTESIAN_POINT('',(0.966370849898476,-1.13137084989848,15.8));
#12605=CARTESIAN_POINT('Origin',(1.13137084989848,-1.13137084989848,16.5));
#12606=CARTESIAN_POINT('Origin',(1.13137084989848,-1.13137084989848,15.8));
#12607=CARTESIAN_POINT('Origin',(-5.23743686707646,-0.9,9.76256313292354));
#12608=CARTESIAN_POINT('',(-5.40243686707646,-0.8,9.76256313292354));
#12609=CARTESIAN_POINT('Origin',(-5.23743686707646,-0.8,9.76256313292354));
#12610=CARTESIAN_POINT('',(-5.40243686707646,0.8,9.76256313292354));
#12611=CARTESIAN_POINT('',(-5.40243686707646,-0.9,9.76256313292354));
#12612=CARTESIAN_POINT('Origin',(-5.23743686707646,0.8,9.76256313292354));
#12613=CARTESIAN_POINT('Origin',(-5.23743686707646,-0.9,12.2374368670765));
#12614=CARTESIAN_POINT('',(-5.40243686707646,-0.8,12.2374368670765));
#12615=CARTESIAN_POINT('Origin',(-5.23743686707646,-0.8,12.2374368670765));
#12616=CARTESIAN_POINT('',(-5.40243686707646,0.8,12.2374368670765));
#12617=CARTESIAN_POINT('',(-5.40243686707646,-0.9,12.2374368670765));
#12618=CARTESIAN_POINT('Origin',(-5.23743686707646,0.8,12.2374368670765));
#12619=CARTESIAN_POINT('Origin',(-2.76256313292354,-0.9,12.2374368670765));
#12620=CARTESIAN_POINT('',(-2.92756313292354,-0.8,12.2374368670765));
#12621=CARTESIAN_POINT('Origin',(-2.76256313292354,-0.8,12.2374368670765));
#12622=CARTESIAN_POINT('',(-2.92756313292354,0.8,12.2374368670765));
#12623=CARTESIAN_POINT('',(-2.92756313292354,-0.9,12.2374368670765));
#12624=CARTESIAN_POINT('Origin',(-2.76256313292354,0.8,12.2374368670765));
#12625=CARTESIAN_POINT('Origin',(-2.76256313292354,-0.9,9.76256313292354));
#12626=CARTESIAN_POINT('',(-2.92756313292354,-0.8,9.76256313292354));
#12627=CARTESIAN_POINT('Origin',(-2.76256313292354,-0.8,9.76256313292354));
#12628=CARTESIAN_POINT('',(-2.92756313292354,0.8,9.76256313292354));
#12629=CARTESIAN_POINT('',(-2.92756313292354,-0.9,9.76256313292354));
#12630=CARTESIAN_POINT('Origin',(-2.76256313292354,0.8,9.76256313292354));
#12631=CARTESIAN_POINT('Origin',(-6.,-1.4,0.9));
#12632=CARTESIAN_POINT('',(-6.275,-1.4,1.));
#12633=CARTESIAN_POINT('Origin',(-6.,-1.4,1.));
#12634=CARTESIAN_POINT('',(-6.275,-1.4,1.8));
#12635=CARTESIAN_POINT('',(-6.275,-1.4,0.9));
#12636=CARTESIAN_POINT('Origin',(-6.,-1.4,1.8));
#12637=CARTESIAN_POINT('Origin',(-8.5,1.4,0.9));
#12638=CARTESIAN_POINT('',(-8.775,1.4,1.));
#12639=CARTESIAN_POINT('Origin',(-8.5,1.4,1.));
#12640=CARTESIAN_POINT('',(-8.775,1.4,1.8));
#12641=CARTESIAN_POINT('',(-8.775,1.4,0.9));
#12642=CARTESIAN_POINT('Origin',(-8.5,1.4,1.8));
#12643=CARTESIAN_POINT('Origin',(-8.5,-1.4,0.9));
#12644=CARTESIAN_POINT('',(-8.775,-1.4,1.));
#12645=CARTESIAN_POINT('Origin',(-8.5,-1.4,1.));
#12646=CARTESIAN_POINT('',(-8.775,-1.4,1.8));
#12647=CARTESIAN_POINT('',(-8.775,-1.4,0.9));
#12648=CARTESIAN_POINT('Origin',(-8.5,-1.4,1.8));
#12649=CARTESIAN_POINT('Origin',(-6.,1.4,0.9));
#12650=CARTESIAN_POINT('',(-6.275,1.4,1.));
#12651=CARTESIAN_POINT('Origin',(-6.,1.4,1.));
#12652=CARTESIAN_POINT('',(-6.275,1.4,1.8));
#12653=CARTESIAN_POINT('',(-6.275,1.4,0.9));
#12654=CARTESIAN_POINT('Origin',(-6.,1.4,1.8));
#12655=CARTESIAN_POINT('Origin',(0.,0.,12.5));
#12656=CARTESIAN_POINT('',(-1.05,-1.28587913910472E-16,12.5));
#12657=CARTESIAN_POINT('Origin',(0.,0.,12.5));
#12658=CARTESIAN_POINT('',(-1.05,1.28587913910472E-16,16.5));
#12659=CARTESIAN_POINT('',(-1.05,-1.28587913910472E-16,12.5));
#12660=CARTESIAN_POINT('Origin',(0.,0.,16.5));
#12661=CARTESIAN_POINT('Origin',(0.,0.,12.5));
#12662=CARTESIAN_POINT('',(-0.625,-7.65404249467096E-17,12.5));
#12663=CARTESIAN_POINT('Origin',(0.,0.,12.5));
#12664=CARTESIAN_POINT('Origin',(0.,0.,11.9));
#12665=CARTESIAN_POINT('',(-0.625,-7.65404249467096E-17,12.));
#12666=CARTESIAN_POINT('Origin',(0.,0.,12.));
#12667=CARTESIAN_POINT('',(-0.625,-7.65404249467096E-17,11.9));
#12668=CARTESIAN_POINT('Origin',(-4.,-0.9,11.));
#12669=CARTESIAN_POINT('',(-5.5,-0.8,11.));
#12670=CARTESIAN_POINT('Origin',(-4.,-0.8,11.));
#12671=CARTESIAN_POINT('',(-5.5,0.8,11.));
#12672=CARTESIAN_POINT('',(-5.5,-0.9,11.));
#12673=CARTESIAN_POINT('Origin',(-4.,0.8,11.));
#12674=CARTESIAN_POINT('Origin',(0.,0.,12.));
#12675=CARTESIAN_POINT('',(-1.83303027798234,-0.8,12.));
#12676=CARTESIAN_POINT('',(-1.83303027798234,-0.8,16.5));
#12677=CARTESIAN_POINT('',(-1.83303027798234,-0.8,12.));
#12678=CARTESIAN_POINT('',(-1.83303027798234,0.8,12.));
#12679=CARTESIAN_POINT('Origin',(0.,0.,12.));
#12680=CARTESIAN_POINT('',(-1.83303027798234,0.8,16.5));
#12681=CARTESIAN_POINT('',(-1.83303027798234,0.8,12.));
#12682=CARTESIAN_POINT('Origin',(0.,0.,16.5));
#12683=CARTESIAN_POINT('Origin',(-8.,-0.8,1.));
#12684=CARTESIAN_POINT('',(-6.5,-0.8,16.5));
#12685=CARTESIAN_POINT('',(1.5,-0.8,16.5));
#12686=CARTESIAN_POINT('',(-6.5,-0.8,17.5));
#12687=CARTESIAN_POINT('',(-6.5,-0.8,1.));
#12688=CARTESIAN_POINT('',(-8.,-0.8,17.5));
#12689=CARTESIAN_POINT('',(-8.,-0.8,17.5));
#12690=CARTESIAN_POINT('',(-8.,-0.8,1.8));
#12691=CARTESIAN_POINT('',(-8.,-0.8,1.));
#12692=CARTESIAN_POINT('',(-6.5,-0.8,1.8));
#12693=CARTESIAN_POINT('',(-7.625,-0.8,1.8));
#12694=CARTESIAN_POINT('',(-6.5,-0.8,12.));
#12695=CARTESIAN_POINT('',(-6.5,-0.8,1.));
#12696=CARTESIAN_POINT('',(-5.95959179422654,-0.8,12.));
#12697=CARTESIAN_POINT('',(-8.,-0.8,12.));
#12698=CARTESIAN_POINT('',(-2.04040820577346,-0.8,12.));
#12699=CARTESIAN_POINT('Origin',(-4.,-0.8,11.));
#12700=CARTESIAN_POINT('',(-8.,-0.8,12.));
#12701=CARTESIAN_POINT('Origin',(-8.,-0.8,16.5));
#12702=CARTESIAN_POINT('',(-6.5,0.8,16.5));
#12703=CARTESIAN_POINT('',(1.5,0.8,16.5));
#12704=CARTESIAN_POINT('',(-6.5,-0.8,16.5));
#12705=CARTESIAN_POINT('Origin',(-7.25,0.,1.8));
#12706=CARTESIAN_POINT('',(-9.,2.,1.8));
#12707=CARTESIAN_POINT('',(-9.,-2.,1.8));
#12708=CARTESIAN_POINT('',(-9.,2.,1.8));
#12709=CARTESIAN_POINT('',(-5.5,-2.,1.8));
#12710=CARTESIAN_POINT('',(-9.,-2.,1.8));
#12711=CARTESIAN_POINT('',(-5.5,2.,1.8));
#12712=CARTESIAN_POINT('',(-5.5,-2.,1.8));
#12713=CARTESIAN_POINT('',(-5.5,2.,1.8));
#12714=CARTESIAN_POINT('',(-6.5,0.8,1.8));
#12715=CARTESIAN_POINT('',(-8.,0.8,1.8));
#12716=CARTESIAN_POINT('',(-6.875,0.8,1.8));
#12717=CARTESIAN_POINT('',(-6.5,-0.4,1.8));
#12718=CARTESIAN_POINT('',(-8.,0.4,1.8));
#12719=CARTESIAN_POINT('Origin',(-5.5,2.,1.));
#12720=CARTESIAN_POINT('',(-5.5,2.,1.));
#12721=CARTESIAN_POINT('',(-9.,2.,1.));
#12722=CARTESIAN_POINT('',(-5.5,2.,1.));
#12723=CARTESIAN_POINT('',(-9.,2.,1.));
#12724=CARTESIAN_POINT('',(-5.5,2.,1.));
#12725=CARTESIAN_POINT('Origin',(-5.5,-2.,1.));
#12726=CARTESIAN_POINT('',(-5.5,-2.,1.));
#12727=CARTESIAN_POINT('',(-5.5,-2.,1.));
#12728=CARTESIAN_POINT('',(-5.5,-2.,1.));
#12729=CARTESIAN_POINT('Origin',(-9.,-2.,1.));
#12730=CARTESIAN_POINT('',(-9.,-2.,1.));
#12731=CARTESIAN_POINT('',(-9.,-2.,1.));
#12732=CARTESIAN_POINT('',(-9.,-2.,1.));
#12733=CARTESIAN_POINT('Origin',(-9.,2.,1.));
#12734=CARTESIAN_POINT('',(-9.,2.,1.));
#12735=CARTESIAN_POINT('Origin',(-6.5,-0.8,1.));
#12736=CARTESIAN_POINT('',(-6.5,0.8,12.));
#12737=CARTESIAN_POINT('',(-6.5,0.8,1.));
#12738=CARTESIAN_POINT('',(-6.5,-0.8,12.));
#12739=CARTESIAN_POINT('Origin',(-4.,-0.8,11.));
#12740=CARTESIAN_POINT('',(-2.04040820577346,0.8,12.));
#12741=CARTESIAN_POINT('',(-2.04040820577346,-0.8,12.));
#12742=CARTESIAN_POINT('',(-5.95959179422654,0.8,12.));
#12743=CARTESIAN_POINT('',(-5.95959179422654,-0.8,12.));
#12744=CARTESIAN_POINT('Origin',(-4.,0.8,11.));
#12745=CARTESIAN_POINT('Origin',(-6.5,0.8,1.));
#12746=CARTESIAN_POINT('',(-8.,0.8,12.));
#12747=CARTESIAN_POINT('',(-8.,0.8,12.));
#12748=CARTESIAN_POINT('',(-8.,0.8,17.5));
#12749=CARTESIAN_POINT('',(-8.,0.8,1.));
#12750=CARTESIAN_POINT('',(-6.5,0.8,17.5));
#12751=CARTESIAN_POINT('',(-6.5,0.8,17.5));
#12752=CARTESIAN_POINT('',(-6.5,0.8,1.));
#12753=CARTESIAN_POINT('Origin',(1.5,-0.8,12.));
#12754=CARTESIAN_POINT('Origin',(1.5,-0.8,12.));
#12755=CARTESIAN_POINT('Origin',(-6.5,-0.8,1.));
#12756=CARTESIAN_POINT('',(-6.5,-0.8,17.5));
#12757=CARTESIAN_POINT('Origin',(-8.,0.8,1.));
#12758=CARTESIAN_POINT('',(-8.,0.8,17.5));
#12759=CARTESIAN_POINT('Origin',(-7.25,0.,17.5));
#12760=CARTESIAN_POINT('Origin',(-7.25,0.,1.));
#12761=CARTESIAN_POINT('',(0.,0.,0.));
#12762=CARTESIAN_POINT('Origin',(-5.23743686707646,-1.1,9.76256313292354));
#12763=CARTESIAN_POINT('',(-5.46243686707646,-1.,9.76256313292354));
#12764=CARTESIAN_POINT('Origin',(-5.23743686707646,-1.,9.76256313292354));
#12765=CARTESIAN_POINT('',(-5.46243686707646,-0.8,9.76256313292354));
#12766=CARTESIAN_POINT('',(-5.46243686707646,-1.1,9.76256313292354));
#12767=CARTESIAN_POINT('Origin',(-5.23743686707646,-0.8,9.76256313292354));
#12768=CARTESIAN_POINT('Origin',(-5.23743686707646,-1.1,12.2374368670765));
#12769=CARTESIAN_POINT('',(-5.46243686707646,-1.,12.2374368670765));
#12770=CARTESIAN_POINT('Origin',(-5.23743686707646,-1.,12.2374368670765));
#12771=CARTESIAN_POINT('',(-5.46243686707646,-0.8,12.2374368670765));
#12772=CARTESIAN_POINT('',(-5.46243686707646,-1.1,12.2374368670765));
#12773=CARTESIAN_POINT('Origin',(-5.23743686707646,-0.8,12.2374368670765));
#12774=CARTESIAN_POINT('Origin',(-2.76256313292354,-1.1,12.2374368670765));
#12775=CARTESIAN_POINT('',(-2.98756313292354,-1.,12.2374368670765));
#12776=CARTESIAN_POINT('Origin',(-2.76256313292354,-1.,12.2374368670765));
#12777=CARTESIAN_POINT('',(-2.98756313292354,-0.8,12.2374368670765));
#12778=CARTESIAN_POINT('',(-2.98756313292354,-1.1,12.2374368670765));
#12779=CARTESIAN_POINT('Origin',(-2.76256313292354,-0.8,12.2374368670765));
#12780=CARTESIAN_POINT('Origin',(-2.76256313292354,-1.1,9.76256313292354));
#12781=CARTESIAN_POINT('',(-2.98756313292354,-1.,9.76256313292354));
#12782=CARTESIAN_POINT('Origin',(-2.76256313292354,-1.,9.76256313292354));
#12783=CARTESIAN_POINT('',(-2.98756313292354,-0.8,9.76256313292354));
#12784=CARTESIAN_POINT('',(-2.98756313292354,-1.1,9.76256313292354));
#12785=CARTESIAN_POINT('Origin',(-2.76256313292354,-0.8,9.76256313292354));
#12786=CARTESIAN_POINT('Origin',(-4.,-0.8,11.));
#12787=CARTESIAN_POINT('',(-5.49,-0.45,11.));
#12788=CARTESIAN_POINT('Origin',(-4.,-0.45,11.));
#12789=CARTESIAN_POINT('',(-5.49,-0.8,11.));
#12790=CARTESIAN_POINT('',(-5.49,-0.8,11.));
#12791=CARTESIAN_POINT('Origin',(-4.,-0.8,11.));
#12792=CARTESIAN_POINT('Origin',(-4.,-0.45,11.));
#12793=CARTESIAN_POINT('',(-4.71,-0.45,11.));
#12794=CARTESIAN_POINT('Origin',(-4.,-0.45,11.));
#12795=CARTESIAN_POINT('Origin',(-4.,-1.,11.));
#12796=CARTESIAN_POINT('',(-4.71,-1.,11.));
#12797=CARTESIAN_POINT('',(-4.71,-1.,11.));
#12798=CARTESIAN_POINT('Origin',(-4.,-1.,11.));
#12799=CARTESIAN_POINT('Origin',(-4.,-1.,11.));
#12800=CARTESIAN_POINT('',(-6.2,-0.8,11.));
#12801=CARTESIAN_POINT('Origin',(-4.,-0.8,11.));
#12802=CARTESIAN_POINT('',(-6.2,-1.,11.));
#12803=CARTESIAN_POINT('',(-6.2,-1.,11.));
#12804=CARTESIAN_POINT('Origin',(-4.,-1.,11.));
#12805=CARTESIAN_POINT('Origin',(-4.,-0.8,11.));
#12806=CARTESIAN_POINT('Origin',(-4.,-1.,11.));
#12807=CARTESIAN_POINT('',(0.,0.,0.));
#12808=CARTESIAN_POINT('Origin',(-5.23743686707646,0.7,9.76256313292354));
#12809=CARTESIAN_POINT('',(-5.46243686707646,0.8,9.76256313292354));
#12810=CARTESIAN_POINT('Origin',(-5.23743686707646,0.8,9.76256313292354));
#12811=CARTESIAN_POINT('',(-5.46243686707646,1.,9.76256313292354));
#12812=CARTESIAN_POINT('',(-5.46243686707646,0.7,9.76256313292354));
#12813=CARTESIAN_POINT('Origin',(-5.23743686707646,1.,9.76256313292354));
#12814=CARTESIAN_POINT('Origin',(-5.23743686707646,0.7,12.2374368670765));
#12815=CARTESIAN_POINT('',(-5.46243686707646,0.8,12.2374368670765));
#12816=CARTESIAN_POINT('Origin',(-5.23743686707646,0.8,12.2374368670765));
#12817=CARTESIAN_POINT('',(-5.46243686707646,1.,12.2374368670765));
#12818=CARTESIAN_POINT('',(-5.46243686707646,0.7,12.2374368670765));
#12819=CARTESIAN_POINT('Origin',(-5.23743686707646,1.,12.2374368670765));
#12820=CARTESIAN_POINT('Origin',(-2.76256313292354,0.7,12.2374368670765));
#12821=CARTESIAN_POINT('',(-2.98756313292354,0.8,12.2374368670765));
#12822=CARTESIAN_POINT('Origin',(-2.76256313292354,0.8,12.2374368670765));
#12823=CARTESIAN_POINT('',(-2.98756313292354,1.,12.2374368670765));
#12824=CARTESIAN_POINT('',(-2.98756313292354,0.7,12.2374368670765));
#12825=CARTESIAN_POINT('Origin',(-2.76256313292354,1.,12.2374368670765));
#12826=CARTESIAN_POINT('Origin',(-2.76256313292354,0.7,9.76256313292354));
#12827=CARTESIAN_POINT('',(-2.98756313292354,0.8,9.76256313292354));
#12828=CARTESIAN_POINT('Origin',(-2.76256313292354,0.8,9.76256313292354));
#12829=CARTESIAN_POINT('',(-2.98756313292354,1.,9.76256313292354));
#12830=CARTESIAN_POINT('',(-2.98756313292354,0.7,9.76256313292354));
#12831=CARTESIAN_POINT('Origin',(-2.76256313292354,1.,9.76256313292354));
#12832=CARTESIAN_POINT('Origin',(-4.,0.45,11.));
#12833=CARTESIAN_POINT('',(-5.49,0.8,11.));
#12834=CARTESIAN_POINT('Origin',(-4.,0.8,11.));
#12835=CARTESIAN_POINT('',(-5.49,0.45,11.));
#12836=CARTESIAN_POINT('',(-5.49,0.45,11.));
#12837=CARTESIAN_POINT('Origin',(-4.,0.45,11.));
#12838=CARTESIAN_POINT('Origin',(-4.,0.45,11.));
#12839=CARTESIAN_POINT('',(-4.71,0.45,11.));
#12840=CARTESIAN_POINT('Origin',(-4.,0.45,11.));
#12841=CARTESIAN_POINT('Origin',(-4.,0.8,11.));
#12842=CARTESIAN_POINT('',(-4.71,1.,11.));
#12843=CARTESIAN_POINT('Origin',(-4.,1.,11.));
#12844=CARTESIAN_POINT('',(-4.71,0.8,11.));
#12845=CARTESIAN_POINT('Origin',(-4.,0.8,11.));
#12846=CARTESIAN_POINT('',(-6.2,1.,11.));
#12847=CARTESIAN_POINT('Origin',(-4.,1.,11.));
#12848=CARTESIAN_POINT('',(-6.2,0.8,11.));
#12849=CARTESIAN_POINT('',(-6.2,0.8,11.));
#12850=CARTESIAN_POINT('Origin',(-4.,0.8,11.));
#12851=CARTESIAN_POINT('Origin',(-4.,1.,11.));
#12852=CARTESIAN_POINT('Origin',(-4.,0.8,11.));
#12853=CARTESIAN_POINT('',(0.,0.,0.));
#12854=CARTESIAN_POINT('Origin',(-1.13137084989848,-1.13137084989848,16.9));
#12855=CARTESIAN_POINT('',(-1.50637084989848,-1.13137084989848,16.9));
#12856=CARTESIAN_POINT('Origin',(-1.13137084989848,-1.13137084989848,16.9));
#12857=CARTESIAN_POINT('',(-1.50637084989848,-1.13137084989848,17.3));
#12858=CARTESIAN_POINT('',(-1.50637084989848,-1.13137084989848,16.9));
#12859=CARTESIAN_POINT('Origin',(-1.13137084989848,-1.13137084989848,17.3));
#12860=CARTESIAN_POINT('Origin',(-1.13137084989848,-1.13137084989848,16.9));
#12861=CARTESIAN_POINT('',(-1.35637084989848,-1.13137084989848,16.9));
#12862=CARTESIAN_POINT('Origin',(-1.13137084989848,-1.13137084989848,16.9));
#12863=CARTESIAN_POINT('Origin',(-1.13137084989848,1.13137084989848,16.9));
#12864=CARTESIAN_POINT('',(-1.50637084989848,1.13137084989848,16.9));
#12865=CARTESIAN_POINT('Origin',(-1.13137084989848,1.13137084989848,16.9));
#12866=CARTESIAN_POINT('',(-1.50637084989848,1.13137084989848,17.3));
#12867=CARTESIAN_POINT('',(-1.50637084989848,1.13137084989848,16.9));
#12868=CARTESIAN_POINT('Origin',(-1.13137084989848,1.13137084989848,17.3));
#12869=CARTESIAN_POINT('Origin',(-1.13137084989848,1.13137084989848,16.9));
#12870=CARTESIAN_POINT('',(-1.35637084989848,1.13137084989848,16.9));
#12871=CARTESIAN_POINT('Origin',(-1.13137084989848,1.13137084989848,16.9));
#12872=CARTESIAN_POINT('Origin',(1.13137084989848,1.13137084989848,16.9));
#12873=CARTESIAN_POINT('',(0.756370849898476,1.13137084989848,16.9));
#12874=CARTESIAN_POINT('Origin',(1.13137084989848,1.13137084989848,16.9));
#12875=CARTESIAN_POINT('',(0.756370849898476,1.13137084989848,17.3));
#12876=CARTESIAN_POINT('',(0.756370849898476,1.13137084989848,16.9));
#12877=CARTESIAN_POINT('Origin',(1.13137084989848,1.13137084989848,17.3));
#12878=CARTESIAN_POINT('Origin',(1.13137084989848,1.13137084989848,16.9));
#12879=CARTESIAN_POINT('',(0.906370849898476,1.13137084989848,16.9));
#12880=CARTESIAN_POINT('Origin',(1.13137084989848,1.13137084989848,16.9));
#12881=CARTESIAN_POINT('Origin',(1.13137084989848,-1.13137084989848,16.9));
#12882=CARTESIAN_POINT('',(0.756370849898476,-1.13137084989848,16.9));
#12883=CARTESIAN_POINT('Origin',(1.13137084989848,-1.13137084989848,16.9));
#12884=CARTESIAN_POINT('',(0.756370849898476,-1.13137084989848,17.3));
#12885=CARTESIAN_POINT('',(0.756370849898476,-1.13137084989848,16.9));
#12886=CARTESIAN_POINT('Origin',(1.13137084989848,-1.13137084989848,17.3));
#12887=CARTESIAN_POINT('Origin',(1.13137084989848,-1.13137084989848,16.9));
#12888=CARTESIAN_POINT('',(0.906370849898476,-1.13137084989848,16.9));
#12889=CARTESIAN_POINT('Origin',(1.13137084989848,-1.13137084989848,16.9));
#12890=CARTESIAN_POINT('Origin',(-1.13137084989848,-1.13137084989848,16.4));
#12891=CARTESIAN_POINT('',(-1.35637084989848,-1.13137084989848,16.5));
#12892=CARTESIAN_POINT('Origin',(-1.13137084989848,-1.13137084989848,16.5));
#12893=CARTESIAN_POINT('',(-1.35637084989848,-1.13137084989848,16.4));
#12894=CARTESIAN_POINT('Origin',(-1.13137084989848,1.13137084989848,16.4));
#12895=CARTESIAN_POINT('',(-1.35637084989848,1.13137084989848,16.5));
#12896=CARTESIAN_POINT('Origin',(-1.13137084989848,1.13137084989848,16.5));
#12897=CARTESIAN_POINT('',(-1.35637084989848,1.13137084989848,16.4));
#12898=CARTESIAN_POINT('Origin',(1.13137084989848,1.13137084989848,16.4));
#12899=CARTESIAN_POINT('',(0.906370849898476,1.13137084989848,16.5));
#12900=CARTESIAN_POINT('Origin',(1.13137084989848,1.13137084989848,16.5));
#12901=CARTESIAN_POINT('',(0.906370849898476,1.13137084989848,16.4));
#12902=CARTESIAN_POINT('Origin',(1.13137084989848,-1.13137084989848,16.4));
#12903=CARTESIAN_POINT('',(0.906370849898476,-1.13137084989848,16.5));
#12904=CARTESIAN_POINT('Origin',(1.13137084989848,-1.13137084989848,16.5));
#12905=CARTESIAN_POINT('',(0.906370849898476,-1.13137084989848,16.4));
#12906=CARTESIAN_POINT('Origin',(0.,0.,15.5));
#12907=CARTESIAN_POINT('',(-1.04,-1.27363267111325E-16,16.5));
#12908=CARTESIAN_POINT('Origin',(0.,0.,16.5));
#12909=CARTESIAN_POINT('',(-1.04,-1.27363267111325E-16,15.5));
#12910=CARTESIAN_POINT('',(-1.04,-1.27363267111325E-16,15.5));
#12911=CARTESIAN_POINT('Origin',(0.,0.,15.5));
#12912=CARTESIAN_POINT('Origin',(0.,0.,15.5));
#12913=CARTESIAN_POINT('',(-0.625,-7.65404249467096E-17,15.5));
#12914=CARTESIAN_POINT('Origin',(0.,0.,15.5));
#12915=CARTESIAN_POINT('Origin',(0.,0.,16.5));
#12916=CARTESIAN_POINT('',(-0.625,-7.65404249467096E-17,17.3));
#12917=CARTESIAN_POINT('Origin',(0.,0.,17.3));
#12918=CARTESIAN_POINT('',(-0.625,-7.65404249467096E-17,16.5));
#12919=CARTESIAN_POINT('Origin',(0.,0.,16.5));
#12920=CARTESIAN_POINT('',(-2.,-2.44929359829471E-16,17.3));
#12921=CARTESIAN_POINT('Origin',(0.,0.,17.3));
#12922=CARTESIAN_POINT('',(-2.,-2.44929359829471E-16,16.5));
#12923=CARTESIAN_POINT('',(-2.,-2.44929359829471E-16,16.5));
#12924=CARTESIAN_POINT('Origin',(0.,0.,16.5));
#12925=CARTESIAN_POINT('Origin',(0.,0.,17.3));
#12926=CARTESIAN_POINT('Origin',(0.,0.,16.5));
#12927=CARTESIAN_POINT('',(0.,0.,0.));
#12928=CARTESIAN_POINT('Origin',(1.,3.5,1.));
#12929=CARTESIAN_POINT('',(1.,3.5,1.));
#12930=CARTESIAN_POINT('',(-1.,3.5,1.));
#12931=CARTESIAN_POINT('',(1.,3.5,1.));
#12932=CARTESIAN_POINT('',(-1.,3.5,3.));
#12933=CARTESIAN_POINT('',(-1.,3.5,1.));
#12934=CARTESIAN_POINT('',(1.,3.5,3.));
#12935=CARTESIAN_POINT('',(1.,3.5,3.));
#12936=CARTESIAN_POINT('',(1.,3.5,1.));
#12937=CARTESIAN_POINT('Origin',(1.,-6.,1.));
#12938=CARTESIAN_POINT('',(1.,-6.,1.));
#12939=CARTESIAN_POINT('',(1.,-6.,1.));
#12940=CARTESIAN_POINT('',(1.,-6.,3.));
#12941=CARTESIAN_POINT('',(1.,-6.,3.));
#12942=CARTESIAN_POINT('',(1.,-6.,1.));
#12943=CARTESIAN_POINT('Origin',(-1.,-6.,1.));
#12944=CARTESIAN_POINT('',(-1.,-6.,1.));
#12945=CARTESIAN_POINT('',(-1.,-6.,1.));
#12946=CARTESIAN_POINT('',(-1.,-6.,3.));
#12947=CARTESIAN_POINT('',(-1.,-6.,3.));
#12948=CARTESIAN_POINT('',(-1.,-6.,1.));
#12949=CARTESIAN_POINT('Origin',(-1.,3.5,1.));
#12950=CARTESIAN_POINT('',(-1.,3.5,1.));
#12951=CARTESIAN_POINT('',(-1.,3.5,3.));
#12952=CARTESIAN_POINT('Origin',(0.,-1.25,3.));
#12953=CARTESIAN_POINT('Origin',(0.,-1.25,1.));
#12954=CARTESIAN_POINT('',(0.,0.,0.));
#12955=CARTESIAN_POINT('Origin',(-1.5,-4.5,0.9));
#12956=CARTESIAN_POINT('',(-1.665,-4.5,1.));
#12957=CARTESIAN_POINT('Origin',(-1.5,-4.5,1.));
#12958=CARTESIAN_POINT('',(-1.665,-4.5,1.7));
#12959=CARTESIAN_POINT('',(-1.665,-4.5,0.9));
#12960=CARTESIAN_POINT('Origin',(-1.5,-4.5,1.7));
#12961=CARTESIAN_POINT('Origin',(-1.5,-4.5,1.7));
#12962=CARTESIAN_POINT('Origin',(-1.5,2.,0.9));
#12963=CARTESIAN_POINT('',(-1.665,2.,1.));
#12964=CARTESIAN_POINT('Origin',(-1.5,2.,1.));
#12965=CARTESIAN_POINT('',(-1.665,2.,1.7));
#12966=CARTESIAN_POINT('',(-1.665,2.,0.9));
#12967=CARTESIAN_POINT('Origin',(-1.5,2.,1.7));
#12968=CARTESIAN_POINT('Origin',(-1.5,2.,1.7));
#12969=CARTESIAN_POINT('Origin',(-1.01,3.5,1.));
#12970=CARTESIAN_POINT('',(-1.01,3.5,1.));
#12971=CARTESIAN_POINT('',(-2.,3.5,1.));
#12972=CARTESIAN_POINT('',(-1.01,3.5,1.));
#12973=CARTESIAN_POINT('',(-2.,3.5,2.5));
#12974=CARTESIAN_POINT('',(-2.,3.5,1.));
#12975=CARTESIAN_POINT('',(-1.01,3.5,2.5));
#12976=CARTESIAN_POINT('',(-1.01,3.5,2.5));
#12977=CARTESIAN_POINT('',(-1.01,3.5,1.));
#12978=CARTESIAN_POINT('Origin',(-1.01,-6.,1.));
#12979=CARTESIAN_POINT('',(-1.01,-6.,1.));
#12980=CARTESIAN_POINT('',(-1.01,-6.,1.));
#12981=CARTESIAN_POINT('',(-1.01,-6.,2.5));
#12982=CARTESIAN_POINT('',(-1.01,-6.,2.5));
#12983=CARTESIAN_POINT('',(-1.01,-6.,1.));
#12984=CARTESIAN_POINT('Origin',(-2.,-6.,1.));
#12985=CARTESIAN_POINT('',(-2.,-6.,1.));
#12986=CARTESIAN_POINT('',(-2.,-6.,1.));
#12987=CARTESIAN_POINT('',(-2.,-6.,2.5));
#12988=CARTESIAN_POINT('',(-2.,-6.,2.5));
#12989=CARTESIAN_POINT('',(-2.,-6.,1.));
#12990=CARTESIAN_POINT('Origin',(-2.,3.5,1.));
#12991=CARTESIAN_POINT('',(-2.,3.5,1.));
#12992=CARTESIAN_POINT('',(-2.,3.5,2.5));
#12993=CARTESIAN_POINT('Origin',(-1.505,-1.25,2.5));
#12994=CARTESIAN_POINT('Origin',(-1.505,-1.25,1.));
#12995=CARTESIAN_POINT('',(0.,0.,0.));
#12996=CARTESIAN_POINT('Origin',(1.5,-4.5,0.9));
#12997=CARTESIAN_POINT('',(1.335,-4.5,1.));
#12998=CARTESIAN_POINT('Origin',(1.5,-4.5,1.));
#12999=CARTESIAN_POINT('',(1.335,-4.5,1.7));
#13000=CARTESIAN_POINT('',(1.335,-4.5,0.9));
#13001=CARTESIAN_POINT('Origin',(1.5,-4.5,1.7));
#13002=CARTESIAN_POINT('Origin',(1.5,-4.5,1.7));
#13003=CARTESIAN_POINT('Origin',(1.5,2.,0.9));
#13004=CARTESIAN_POINT('',(1.335,2.,1.));
#13005=CARTESIAN_POINT('Origin',(1.5,2.,1.));
#13006=CARTESIAN_POINT('',(1.335,2.,1.7));
#13007=CARTESIAN_POINT('',(1.335,2.,0.9));
#13008=CARTESIAN_POINT('Origin',(1.5,2.,1.7));
#13009=CARTESIAN_POINT('Origin',(1.5,2.,1.7));
#13010=CARTESIAN_POINT('Origin',(2.,3.5,1.));
#13011=CARTESIAN_POINT('',(2.,3.5,1.));
#13012=CARTESIAN_POINT('',(1.01,3.5,1.));
#13013=CARTESIAN_POINT('',(2.,3.5,1.));
#13014=CARTESIAN_POINT('',(1.01,3.5,2.5));
#13015=CARTESIAN_POINT('',(1.01,3.5,1.));
#13016=CARTESIAN_POINT('',(2.,3.5,2.5));
#13017=CARTESIAN_POINT('',(2.,3.5,2.5));
#13018=CARTESIAN_POINT('',(2.,3.5,1.));
#13019=CARTESIAN_POINT('Origin',(2.,-6.,1.));
#13020=CARTESIAN_POINT('',(2.,-6.,1.));
#13021=CARTESIAN_POINT('',(2.,-6.,1.));
#13022=CARTESIAN_POINT('',(2.,-6.,2.5));
#13023=CARTESIAN_POINT('',(2.,-6.,2.5));
#13024=CARTESIAN_POINT('',(2.,-6.,1.));
#13025=CARTESIAN_POINT('Origin',(1.01,-6.,1.));
#13026=CARTESIAN_POINT('',(1.01,-6.,1.));
#13027=CARTESIAN_POINT('',(1.01,-6.,1.));
#13028=CARTESIAN_POINT('',(1.01,-6.,2.5));
#13029=CARTESIAN_POINT('',(1.01,-6.,2.5));
#13030=CARTESIAN_POINT('',(1.01,-6.,1.));
#13031=CARTESIAN_POINT('Origin',(1.01,3.5,1.));
#13032=CARTESIAN_POINT('',(1.01,3.5,1.));
#13033=CARTESIAN_POINT('',(1.01,3.5,2.5));
#13034=CARTESIAN_POINT('Origin',(1.505,-1.25,2.5));
#13035=CARTESIAN_POINT('Origin',(1.505,-1.25,1.));
#13036=CARTESIAN_POINT('',(0.,0.,0.));
#13037=CARTESIAN_POINT('Origin',(-5.25982293614231,-2.4,14.8604204653858));
#13038=CARTESIAN_POINT('',(-5.42482293614231,-2.4,14.8604204653858));
#13039=CARTESIAN_POINT('Origin',(-5.25982293614231,-2.4,14.8604204653858));
#13040=CARTESIAN_POINT('',(-5.42482293614231,-0.8,14.8604204653858));
#13041=CARTESIAN_POINT('',(-5.42482293614231,-2.4,14.8604204653858));
#13042=CARTESIAN_POINT('Origin',(-5.25982293614231,-0.8,14.8604204653858));
#13043=CARTESIAN_POINT('Origin',(-5.25982293614231,-2.4,14.8604204653858));
#13044=CARTESIAN_POINT('Origin',(-5.25982293614231,-2.3,14.8604204653858));
#13045=CARTESIAN_POINT('',(-5.75982293614231,-2.3,14.8604204653858));
#13046=CARTESIAN_POINT('Origin',(-5.25982293614231,-2.3,14.8604204653858));
#13047=CARTESIAN_POINT('',(-5.55982293614231,-2.3,14.8604204653858));
#13048=CARTESIAN_POINT('Origin',(-5.25982293614231,-2.3,14.8604204653858));
#13049=CARTESIAN_POINT('Origin',(-5.25982293614231,-2.3,14.8604204653858));
#13050=CARTESIAN_POINT('',(-5.75982293614231,-0.8,14.8604204653858));
#13051=CARTESIAN_POINT('Origin',(-5.25982293614231,-0.8,14.8604204653858));
#13052=CARTESIAN_POINT('',(-5.75982293614231,-2.3,14.8604204653858));
#13053=CARTESIAN_POINT('Origin',(-5.25982293614231,-0.8,14.8604204653858));
#13054=CARTESIAN_POINT('Origin',(-5.25982293614231,-3.9,14.8604204653858));
#13055=CARTESIAN_POINT('',(-5.55982293614231,-3.9,14.8604204653858));
#13056=CARTESIAN_POINT('',(-5.55982293614231,-3.9,14.8604204653858));
#13057=CARTESIAN_POINT('Origin',(-5.25982293614231,-3.9,14.8604204653858));
#13058=CARTESIAN_POINT('Origin',(-5.25982293614231,-3.9,14.8604204653858));
#13059=CARTESIAN_POINT('',(0.,0.,0.));
#13060=CARTESIAN_POINT('Origin',(-0.1,0.82,-0.3));
#13061=CARTESIAN_POINT('',(0.,0.82,-0.3));
#13062=CARTESIAN_POINT('',(0.,1.,-0.3));
#13063=CARTESIAN_POINT('',(0.,0.41,-0.3));
#13064=CARTESIAN_POINT('',(20.,0.82,-0.3));
#13065=CARTESIAN_POINT('',(-0.1,0.82,-0.3));
#13066=CARTESIAN_POINT('',(20.,1.,-0.3));
#13067=CARTESIAN_POINT('',(20.,0.41,-0.3));
#13068=CARTESIAN_POINT('',(-0.05,1.,-0.3));
#13069=CARTESIAN_POINT('Origin',(-0.1,0.82,-0.55));
#13070=CARTESIAN_POINT('',(0.,0.82,-0.55));
#13071=CARTESIAN_POINT('',(0.,0.82,-0.275));
#13072=CARTESIAN_POINT('',(20.,0.82,-0.55));
#13073=CARTESIAN_POINT('',(-0.1,0.82,-0.55));
#13074=CARTESIAN_POINT('',(20.,0.82,-0.275));
#13075=CARTESIAN_POINT('Origin',(-0.1,0.67,-0.55));
#13076=CARTESIAN_POINT('',(0.,0.67,-0.55));
#13077=CARTESIAN_POINT('',(0.,0.335,-0.55));
#13078=CARTESIAN_POINT('',(20.,0.67,-0.55));
#13079=CARTESIAN_POINT('',(-0.1,0.67,-0.55));
#13080=CARTESIAN_POINT('',(20.,0.335,-0.55));
#13081=CARTESIAN_POINT('Origin',(-0.1,0.42,-0.3));
#13082=CARTESIAN_POINT('',(0.,0.42,-0.3));
#13083=CARTESIAN_POINT('',(0.,0.24,-0.12));
#13084=CARTESIAN_POINT('',(20.,0.42,-0.3));
#13085=CARTESIAN_POINT('',(-0.1,0.42,-0.3));
#13086=CARTESIAN_POINT('',(20.,0.24,-0.12));
#13087=CARTESIAN_POINT('Origin',(-0.1,0.42,0.3));
#13088=CARTESIAN_POINT('',(0.,0.42,0.3));
#13089=CARTESIAN_POINT('',(0.,0.42,0.15));
#13090=CARTESIAN_POINT('',(20.,0.42,0.3));
#13091=CARTESIAN_POINT('',(-0.1,0.42,0.3));
#13092=CARTESIAN_POINT('',(20.,0.42,0.15));
#13093=CARTESIAN_POINT('Origin',(-0.1,0.67,0.55));
#13094=CARTESIAN_POINT('',(0.,0.67,0.55));
#13095=CARTESIAN_POINT('',(6.93889390390723E-18,0.365,0.245));
#13096=CARTESIAN_POINT('',(20.,0.67,0.55));
#13097=CARTESIAN_POINT('',(-0.1,0.67,0.55));
#13098=CARTESIAN_POINT('',(20.,0.365,0.245));
#13099=CARTESIAN_POINT('Origin',(-0.1,0.82,0.55));
#13100=CARTESIAN_POINT('',(0.,0.82,0.55));
#13101=CARTESIAN_POINT('',(0.,0.41,0.55));
#13102=CARTESIAN_POINT('',(20.,0.82,0.55));
#13103=CARTESIAN_POINT('',(-0.1,0.82,0.55));
#13104=CARTESIAN_POINT('',(20.,0.41,0.55));
#13105=CARTESIAN_POINT('Origin',(-0.1,0.82,0.3));
#13106=CARTESIAN_POINT('',(0.,0.82,0.3));
#13107=CARTESIAN_POINT('',(0.,0.82,0.15));
#13108=CARTESIAN_POINT('',(20.,0.82,0.3));
#13109=CARTESIAN_POINT('',(-0.1,0.82,0.3));
#13110=CARTESIAN_POINT('',(20.,0.82,0.15));
#13111=CARTESIAN_POINT('Origin',(-0.1,1.05,0.3));
#13112=CARTESIAN_POINT('',(0.,1.,0.3));
#13113=CARTESIAN_POINT('',(0.,0.525,0.3));
#13114=CARTESIAN_POINT('',(20.,1.,0.3));
#13115=CARTESIAN_POINT('',(-0.05,1.,0.3));
#13116=CARTESIAN_POINT('',(20.,0.525,0.3));
#13117=CARTESIAN_POINT('Origin',(-0.1,-0.3,-0.82));
#13118=CARTESIAN_POINT('',(0.,-0.3,-0.82));
#13119=CARTESIAN_POINT('',(0.,-0.3,-1.));
#13120=CARTESIAN_POINT('',(0.,-0.3,-0.41));
#13121=CARTESIAN_POINT('',(20.,-0.3,-0.82));
#13122=CARTESIAN_POINT('',(-0.1,-0.3,-0.82));
#13123=CARTESIAN_POINT('',(20.,-0.3,-1.));
#13124=CARTESIAN_POINT('',(20.,-0.3,-0.41));
#13125=CARTESIAN_POINT('',(-0.05,-0.3,-1.));
#13126=CARTESIAN_POINT('Origin',(-0.1,-0.55,-0.82));
#13127=CARTESIAN_POINT('',(0.,-0.55,-0.82));
#13128=CARTESIAN_POINT('',(0.,-0.275,-0.82));
#13129=CARTESIAN_POINT('',(20.,-0.55,-0.82));
#13130=CARTESIAN_POINT('',(-0.1,-0.55,-0.82));
#13131=CARTESIAN_POINT('',(20.,-0.275,-0.82));
#13132=CARTESIAN_POINT('Origin',(-0.1,-0.55,-0.67));
#13133=CARTESIAN_POINT('',(0.,-0.55,-0.67));
#13134=CARTESIAN_POINT('',(0.,-0.55,-0.335));
#13135=CARTESIAN_POINT('',(20.,-0.55,-0.67));
#13136=CARTESIAN_POINT('',(-0.1,-0.55,-0.67));
#13137=CARTESIAN_POINT('',(20.,-0.55,-0.335));
#13138=CARTESIAN_POINT('Origin',(-0.1,-0.3,-0.42));
#13139=CARTESIAN_POINT('',(0.,-0.3,-0.42));
#13140=CARTESIAN_POINT('',(0.,-0.12,-0.24));
#13141=CARTESIAN_POINT('',(20.,-0.3,-0.42));
#13142=CARTESIAN_POINT('',(-0.1,-0.3,-0.42));
#13143=CARTESIAN_POINT('',(20.,-0.12,-0.24));
#13144=CARTESIAN_POINT('Origin',(-0.1,0.3,-0.42));
#13145=CARTESIAN_POINT('',(0.,0.3,-0.42));
#13146=CARTESIAN_POINT('',(0.,0.15,-0.42));
#13147=CARTESIAN_POINT('',(20.,0.3,-0.42));
#13148=CARTESIAN_POINT('',(-0.1,0.3,-0.42));
#13149=CARTESIAN_POINT('',(20.,0.15,-0.42));
#13150=CARTESIAN_POINT('Origin',(-0.1,0.55,-0.67));
#13151=CARTESIAN_POINT('',(0.,0.55,-0.67));
#13152=CARTESIAN_POINT('',(0.,0.245,-0.365));
#13153=CARTESIAN_POINT('',(20.,0.55,-0.67));
#13154=CARTESIAN_POINT('',(-0.1,0.55,-0.67));
#13155=CARTESIAN_POINT('',(20.,0.245,-0.365));
#13156=CARTESIAN_POINT('Origin',(-0.1,0.55,-0.82));
#13157=CARTESIAN_POINT('',(0.,0.55,-0.82));
#13158=CARTESIAN_POINT('',(0.,0.55,-0.41));
#13159=CARTESIAN_POINT('',(20.,0.55,-0.82));
#13160=CARTESIAN_POINT('',(-0.1,0.55,-0.82));
#13161=CARTESIAN_POINT('',(20.,0.55,-0.41));
#13162=CARTESIAN_POINT('Origin',(-0.1,0.3,-0.82));
#13163=CARTESIAN_POINT('',(0.,0.3,-0.82));
#13164=CARTESIAN_POINT('',(0.,0.15,-0.82));
#13165=CARTESIAN_POINT('',(20.,0.3,-0.82));
#13166=CARTESIAN_POINT('',(-0.1,0.3,-0.82));
#13167=CARTESIAN_POINT('',(20.,0.15,-0.82));
#13168=CARTESIAN_POINT('Origin',(-0.1,0.3,-1.05));
#13169=CARTESIAN_POINT('',(0.,0.3,-1.));
#13170=CARTESIAN_POINT('',(0.,0.3,-0.525));
#13171=CARTESIAN_POINT('',(20.,0.3,-1.));
#13172=CARTESIAN_POINT('',(-0.05,0.3,-1.));
#13173=CARTESIAN_POINT('',(20.,0.3,-0.525));
#13174=CARTESIAN_POINT('Origin',(-0.1,-0.82,0.3));
#13175=CARTESIAN_POINT('',(0.,-0.82,0.3));
#13176=CARTESIAN_POINT('',(0.,-1.,0.3));
#13177=CARTESIAN_POINT('',(0.,-0.41,0.3));
#13178=CARTESIAN_POINT('',(20.,-0.82,0.3));
#13179=CARTESIAN_POINT('',(-0.1,-0.82,0.3));
#13180=CARTESIAN_POINT('',(20.,-1.,0.3));
#13181=CARTESIAN_POINT('',(20.,-0.41,0.3));
#13182=CARTESIAN_POINT('',(-0.05,-1.,0.3));
#13183=CARTESIAN_POINT('Origin',(-0.1,-0.82,0.55));
#13184=CARTESIAN_POINT('',(0.,-0.82,0.55));
#13185=CARTESIAN_POINT('',(0.,-0.82,0.275));
#13186=CARTESIAN_POINT('',(20.,-0.82,0.55));
#13187=CARTESIAN_POINT('',(-0.1,-0.82,0.55));
#13188=CARTESIAN_POINT('',(20.,-0.82,0.275));
#13189=CARTESIAN_POINT('Origin',(-0.1,-0.67,0.55));
#13190=CARTESIAN_POINT('',(0.,-0.67,0.55));
#13191=CARTESIAN_POINT('',(0.,-0.335,0.55));
#13192=CARTESIAN_POINT('',(20.,-0.67,0.55));
#13193=CARTESIAN_POINT('',(-0.1,-0.67,0.55));
#13194=CARTESIAN_POINT('',(20.,-0.335,0.55));
#13195=CARTESIAN_POINT('Origin',(-0.1,-0.42,0.3));
#13196=CARTESIAN_POINT('',(0.,-0.42,0.3));
#13197=CARTESIAN_POINT('',(-6.93889390390723E-18,-0.24,0.12));
#13198=CARTESIAN_POINT('',(20.,-0.42,0.3));
#13199=CARTESIAN_POINT('',(-0.1,-0.42,0.3));
#13200=CARTESIAN_POINT('',(20.,-0.24,0.12));
#13201=CARTESIAN_POINT('Origin',(-0.1,-0.42,-0.3));
#13202=CARTESIAN_POINT('',(0.,-0.42,-0.3));
#13203=CARTESIAN_POINT('',(0.,-0.42,-0.15));
#13204=CARTESIAN_POINT('',(20.,-0.42,-0.3));
#13205=CARTESIAN_POINT('',(-0.1,-0.42,-0.3));
#13206=CARTESIAN_POINT('',(20.,-0.42,-0.15));
#13207=CARTESIAN_POINT('Origin',(-0.1,-0.67,-0.55));
#13208=CARTESIAN_POINT('',(0.,-0.67,-0.55));
#13209=CARTESIAN_POINT('',(0.,-0.365,-0.245));
#13210=CARTESIAN_POINT('',(20.,-0.67,-0.55));
#13211=CARTESIAN_POINT('',(-0.1,-0.67,-0.55));
#13212=CARTESIAN_POINT('',(20.,-0.365,-0.245));
#13213=CARTESIAN_POINT('Origin',(-0.1,-0.82,-0.55));
#13214=CARTESIAN_POINT('',(0.,-0.82,-0.55));
#13215=CARTESIAN_POINT('',(0.,-0.41,-0.55));
#13216=CARTESIAN_POINT('',(20.,-0.82,-0.55));
#13217=CARTESIAN_POINT('',(-0.1,-0.82,-0.55));
#13218=CARTESIAN_POINT('',(20.,-0.41,-0.55));
#13219=CARTESIAN_POINT('Origin',(-0.1,-0.82,-0.3));
#13220=CARTESIAN_POINT('',(0.,-0.82,-0.3));
#13221=CARTESIAN_POINT('',(0.,-0.82,-0.15));
#13222=CARTESIAN_POINT('',(20.,-0.82,-0.3));
#13223=CARTESIAN_POINT('',(-0.1,-0.82,-0.3));
#13224=CARTESIAN_POINT('',(20.,-0.82,-0.15));
#13225=CARTESIAN_POINT('Origin',(-0.1,-1.05,-0.3));
#13226=CARTESIAN_POINT('',(0.,-1.,-0.3));
#13227=CARTESIAN_POINT('',(0.,-0.525,-0.3));
#13228=CARTESIAN_POINT('',(20.,-1.,-0.3));
#13229=CARTESIAN_POINT('',(-0.05,-1.,-0.3));
#13230=CARTESIAN_POINT('',(20.,-0.525,-0.3));
#13231=CARTESIAN_POINT('Origin',(-0.1,0.3,0.82));
#13232=CARTESIAN_POINT('',(0.,0.3,0.82));
#13233=CARTESIAN_POINT('',(0.,0.3,1.));
#13234=CARTESIAN_POINT('',(0.,0.3,0.41));
#13235=CARTESIAN_POINT('',(20.,0.3,0.82));
#13236=CARTESIAN_POINT('',(-0.1,0.3,0.82));
#13237=CARTESIAN_POINT('',(20.,0.3,1.));
#13238=CARTESIAN_POINT('',(20.,0.3,0.41));
#13239=CARTESIAN_POINT('',(-0.05,0.3,1.));
#13240=CARTESIAN_POINT('Origin',(-0.1,0.55,0.82));
#13241=CARTESIAN_POINT('',(0.,0.55,0.82));
#13242=CARTESIAN_POINT('',(0.,0.275,0.82));
#13243=CARTESIAN_POINT('',(20.,0.55,0.82));
#13244=CARTESIAN_POINT('',(-0.1,0.55,0.82));
#13245=CARTESIAN_POINT('',(20.,0.275,0.82));
#13246=CARTESIAN_POINT('Origin',(-0.1,0.55,0.67));
#13247=CARTESIAN_POINT('',(0.,0.55,0.67));
#13248=CARTESIAN_POINT('',(0.,0.55,0.335));
#13249=CARTESIAN_POINT('',(20.,0.55,0.67));
#13250=CARTESIAN_POINT('',(-0.1,0.55,0.67));
#13251=CARTESIAN_POINT('',(20.,0.55,0.335));
#13252=CARTESIAN_POINT('Origin',(-0.1,0.3,0.42));
#13253=CARTESIAN_POINT('',(0.,0.3,0.42));
#13254=CARTESIAN_POINT('',(6.93889390390723E-18,0.12,0.24));
#13255=CARTESIAN_POINT('',(20.,0.3,0.42));
#13256=CARTESIAN_POINT('',(-0.1,0.3,0.42));
#13257=CARTESIAN_POINT('',(20.,0.12,0.24));
#13258=CARTESIAN_POINT('Origin',(-0.1,-0.3,0.42));
#13259=CARTESIAN_POINT('',(0.,-0.3,0.42));
#13260=CARTESIAN_POINT('',(0.,-0.15,0.42));
#13261=CARTESIAN_POINT('',(20.,-0.3,0.42));
#13262=CARTESIAN_POINT('',(-0.1,-0.3,0.42));
#13263=CARTESIAN_POINT('',(20.,-0.15,0.42));
#13264=CARTESIAN_POINT('Origin',(-0.1,-0.55,0.67));
#13265=CARTESIAN_POINT('',(0.,-0.55,0.67));
#13266=CARTESIAN_POINT('',(6.93889390390723E-18,-0.245,0.365));
#13267=CARTESIAN_POINT('',(20.,-0.55,0.67));
#13268=CARTESIAN_POINT('',(-0.1,-0.55,0.67));
#13269=CARTESIAN_POINT('',(20.,-0.245,0.365));
#13270=CARTESIAN_POINT('Origin',(-0.1,-0.55,0.82));
#13271=CARTESIAN_POINT('',(0.,-0.55,0.82));
#13272=CARTESIAN_POINT('',(0.,-0.55,0.41));
#13273=CARTESIAN_POINT('',(20.,-0.55,0.82));
#13274=CARTESIAN_POINT('',(-0.1,-0.55,0.82));
#13275=CARTESIAN_POINT('',(20.,-0.55,0.41));
#13276=CARTESIAN_POINT('Origin',(-0.1,-0.3,0.82));
#13277=CARTESIAN_POINT('',(0.,-0.3,0.82));
#13278=CARTESIAN_POINT('',(0.,-0.15,0.82));
#13279=CARTESIAN_POINT('',(20.,-0.3,0.82));
#13280=CARTESIAN_POINT('',(-0.1,-0.3,0.82));
#13281=CARTESIAN_POINT('',(20.,-0.15,0.82));
#13282=CARTESIAN_POINT('Origin',(-0.1,-0.3,1.05));
#13283=CARTESIAN_POINT('',(0.,-0.3,1.));
#13284=CARTESIAN_POINT('',(0.,-0.3,0.525));
#13285=CARTESIAN_POINT('',(20.,-0.3,1.));
#13286=CARTESIAN_POINT('',(-0.05,-0.3,1.));
#13287=CARTESIAN_POINT('',(20.,-0.3,0.525));
#13288=CARTESIAN_POINT('Origin',(-0.1,0.,0.));
#13289=CARTESIAN_POINT('',(0.,-2.57175827820944E-17,0.21));
#13290=CARTESIAN_POINT('Origin',(0.,0.,0.));
#13291=CARTESIAN_POINT('',(20.,2.57175827820944E-17,0.21));
#13292=CARTESIAN_POINT('',(-0.1,-2.57175827820944E-17,0.21));
#13293=CARTESIAN_POINT('Origin',(20.,0.,0.));
#13294=CARTESIAN_POINT('Origin',(0.,1.,-1.));
#13295=CARTESIAN_POINT('',(0.,1.,1.));
#13296=CARTESIAN_POINT('',(0.,1.,-1.));
#13297=CARTESIAN_POINT('',(20.,1.,1.));
#13298=CARTESIAN_POINT('',(0.,1.,1.));
#13299=CARTESIAN_POINT('',(20.,1.,-1.));
#13300=CARTESIAN_POINT('Origin',(0.,1.,-1.));
#13301=CARTESIAN_POINT('',(20.,1.,-1.));
#13302=CARTESIAN_POINT('',(20.,1.,-1.));
#13303=CARTESIAN_POINT('',(0.,1.,-1.));
#13304=CARTESIAN_POINT('',(0.,1.,-1.));
#13305=CARTESIAN_POINT('',(0.,1.,-1.));
#13306=CARTESIAN_POINT('Origin',(0.,-1.,-1.));
#13307=CARTESIAN_POINT('',(0.,-1.,-1.));
#13308=CARTESIAN_POINT('',(20.,-1.,-1.));
#13309=CARTESIAN_POINT('Origin',(0.,-1.,-1.));
#13310=CARTESIAN_POINT('',(20.,-1.,-1.));
#13311=CARTESIAN_POINT('',(20.,-1.,-1.));
#13312=CARTESIAN_POINT('',(0.,-1.,-1.));
#13313=CARTESIAN_POINT('',(0.,-1.,-1.));
#13314=CARTESIAN_POINT('',(0.,-1.,-1.));
#13315=CARTESIAN_POINT('Origin',(0.,-1.,1.));
#13316=CARTESIAN_POINT('',(0.,-1.,1.));
#13317=CARTESIAN_POINT('',(20.,-1.,1.));
#13318=CARTESIAN_POINT('Origin',(0.,-1.,1.));
#13319=CARTESIAN_POINT('',(20.,-1.,1.));
#13320=CARTESIAN_POINT('',(20.,-1.,1.));
#13321=CARTESIAN_POINT('',(0.,-1.,1.));
#13322=CARTESIAN_POINT('',(0.,-1.,1.));
#13323=CARTESIAN_POINT('',(0.,-1.,1.));
#13324=CARTESIAN_POINT('Origin',(0.,1.,1.));
#13325=CARTESIAN_POINT('',(0.,1.,1.));
#13326=CARTESIAN_POINT('',(20.,1.,1.));
#13327=CARTESIAN_POINT('Origin',(0.,1.,1.));
#13328=CARTESIAN_POINT('',(20.,1.,1.));
#13329=CARTESIAN_POINT('',(0.,1.,1.));
#13330=CARTESIAN_POINT('Origin',(20.,0.,0.));
#13331=CARTESIAN_POINT('Origin',(0.,0.,0.));
#13332=CARTESIAN_POINT('',(0.,0.,0.));
#13333=CARTESIAN_POINT('Origin',(0.,0.395,0.25));
#13334=CARTESIAN_POINT('',(-0.5,0.3,0.25));
#13335=CARTESIAN_POINT('',(0.5,0.3,0.25));
#13336=CARTESIAN_POINT('',(0.25,0.3,0.25));
#13337=CARTESIAN_POINT('',(-0.5,0.5,0.25));
#13338=CARTESIAN_POINT('',(-0.5,0.5,0.25));
#13339=CARTESIAN_POINT('',(0.5,0.5,0.25));
#13340=CARTESIAN_POINT('',(0.5,0.5,0.25));
#13341=CARTESIAN_POINT('',(0.5,0.29,0.25));
#13342=CARTESIAN_POINT('Origin',(0.5,0.5,0.25));
#13343=CARTESIAN_POINT('',(-0.5,0.5,0.4));
#13344=CARTESIAN_POINT('',(-0.5,0.5,0.25));
#13345=CARTESIAN_POINT('',(0.5,0.5,0.4));
#13346=CARTESIAN_POINT('',(0.5,0.5,0.4));
#13347=CARTESIAN_POINT('',(0.5,0.5,0.25));
#13348=CARTESIAN_POINT('Origin',(0.,0.,0.4));
#13349=CARTESIAN_POINT('',(-0.5,-0.5,0.4));
#13350=CARTESIAN_POINT('',(-0.5,0.5,0.4));
#13351=CARTESIAN_POINT('',(0.5,-0.5,0.4));
#13352=CARTESIAN_POINT('',(-0.5,-0.5,0.4));
#13353=CARTESIAN_POINT('',(0.5,-0.3,0.4));
#13354=CARTESIAN_POINT('',(-0.2117,2.59257727379495E-17,0.4));
#13355=CARTESIAN_POINT('Origin',(0.,0.,0.4));
#13356=CARTESIAN_POINT('Origin',(-0.5,0.3,0.));
#13357=CARTESIAN_POINT('',(-0.5,0.3,0.15));
#13358=CARTESIAN_POINT('',(-0.5,0.3,0.));
#13359=CARTESIAN_POINT('',(-0.5,0.15,0.));
#13360=CARTESIAN_POINT('',(-0.5,0.225,0.075));
#13361=CARTESIAN_POINT('',(-0.5,-0.15,0.));
#13362=CARTESIAN_POINT('',(-0.5,0.3,0.));
#13363=CARTESIAN_POINT('',(-0.5,-0.3,0.15));
#13364=CARTESIAN_POINT('',(-0.5,-0.075,-0.075));
#13365=CARTESIAN_POINT('',(-0.5,-0.3,0.25));
#13366=CARTESIAN_POINT('',(-0.5,-0.3,0.));
#13367=CARTESIAN_POINT('',(-0.5,-0.5,0.25));
#13368=CARTESIAN_POINT('',(-0.5,-0.29,0.25));
#13369=CARTESIAN_POINT('',(-0.5,-0.5,0.25));
#13370=CARTESIAN_POINT('Origin',(-0.5,-0.5,0.25));
#13371=CARTESIAN_POINT('',(0.5,-0.5,0.25));
#13372=CARTESIAN_POINT('',(-0.5,-0.5,0.25));
#13373=CARTESIAN_POINT('',(0.5,-0.5,0.25));
#13374=CARTESIAN_POINT('Origin',(0.,-0.395,0.25));
#13375=CARTESIAN_POINT('',(0.5,-0.3,0.25));
#13376=CARTESIAN_POINT('',(-0.25,-0.3,0.25));
#13377=CARTESIAN_POINT('',(0.5,-0.5,0.25));
#13378=CARTESIAN_POINT('Origin',(0.5,-0.3,0.));
#13379=CARTESIAN_POINT('',(0.5,-0.3,0.15));
#13380=CARTESIAN_POINT('',(0.5,-0.3,0.));
#13381=CARTESIAN_POINT('',(0.5,-0.15,0.));
#13382=CARTESIAN_POINT('',(0.5,-0.225,0.075));
#13383=CARTESIAN_POINT('',(0.5,0.15,0.));
#13384=CARTESIAN_POINT('',(0.5,-0.3,0.));
#13385=CARTESIAN_POINT('',(0.5,0.3,0.15));
#13386=CARTESIAN_POINT('',(0.5,0.075,-0.075));
#13387=CARTESIAN_POINT('',(0.5,0.3,0.));
#13388=CARTESIAN_POINT('Origin',(-0.5,-0.3,0.));
#13389=CARTESIAN_POINT('',(-0.25,-0.3,0.15));
#13390=CARTESIAN_POINT('Origin',(-0.25,-0.225,0.075));
#13391=CARTESIAN_POINT('',(-0.149388386429468,-0.15,0.));
#13392=CARTESIAN_POINT('',(-0.25,-0.15,0.));
#13393=CARTESIAN_POINT('',(0.149388386429468,-0.15,0.));
#13394=CARTESIAN_POINT('Origin',(0.,0.,-0.15));
#13395=CARTESIAN_POINT('',(-0.25,-0.15,0.));
#13396=CARTESIAN_POINT('Origin',(0.,0.,-0.1));
#13397=CARTESIAN_POINT('',(-0.2117,-2.59257727379495E-17,0.));
#13398=CARTESIAN_POINT('Origin',(0.,0.,0.));
#13399=CARTESIAN_POINT('',(-0.2117,-2.59257727379495E-17,-0.1));
#13400=CARTESIAN_POINT('',(-0.149388386429468,0.15,0.));
#13401=CARTESIAN_POINT('Origin',(0.,0.,0.));
#13402=CARTESIAN_POINT('',(0.149388386429468,0.15,0.));
#13403=CARTESIAN_POINT('Origin',(0.,0.,-0.15));
#13404=CARTESIAN_POINT('Origin',(0.,0.,0.));
#13405=CARTESIAN_POINT('Origin',(0.,0.,0.));
#13406=CARTESIAN_POINT('',(0.25,0.15,0.));
#13407=CARTESIAN_POINT('Origin',(0.,0.,0.));
#13408=CARTESIAN_POINT('',(0.25,0.15,0.));
#13409=CARTESIAN_POINT('Origin',(0.25,0.225,0.075));
#13410=CARTESIAN_POINT('',(0.25,0.3,0.15));
#13411=CARTESIAN_POINT('Origin',(0.5,0.3,0.));
#13412=CARTESIAN_POINT('',(0.,0.,0.));
#13413=CARTESIAN_POINT('Origin',(0.,0.09,0.));
#13414=CARTESIAN_POINT('',(-0.285,0.1,3.49024337756996E-17));
#13415=CARTESIAN_POINT('Origin',(0.,0.1,0.));
#13416=CARTESIAN_POINT('',(-0.265,0.08,-3.24531401774049E-17));
#13417=CARTESIAN_POINT('',(-0.275,0.09,3.36777869765522E-17));
#13418=CARTESIAN_POINT('Origin',(0.,0.08,0.));
#13419=CARTESIAN_POINT('Origin',(0.,0.,0.));
#13420=CARTESIAN_POINT('',(-0.265,0.,3.24531401774049E-17));
#13421=CARTESIAN_POINT('',(-0.265,0.,3.24531401774049E-17));
#13422=CARTESIAN_POINT('Origin',(0.,0.,0.));
#13423=CARTESIAN_POINT('Origin',(0.,0.1,0.));
#13424=CARTESIAN_POINT('',(-0.5,0.1,6.12323399573677E-17));
#13425=CARTESIAN_POINT('Origin',(0.,0.1,0.));
#13426=CARTESIAN_POINT('Origin',(0.,0.,0.));
#13427=CARTESIAN_POINT('',(-0.5,0.,6.12323399573677E-17));
#13428=CARTESIAN_POINT('',(-0.5,0.,6.12323399573677E-17));
#13429=CARTESIAN_POINT('Origin',(0.,0.,0.));
#13430=CARTESIAN_POINT('Origin',(0.,0.,0.));
#13431=CARTESIAN_POINT('',(0.,0.,0.));
#13432=CARTESIAN_POINT('Origin',(0.115470053837925,-0.5,-0.2));
#13433=CARTESIAN_POINT('',(0.23094010767585,-0.5,0.));
#13434=CARTESIAN_POINT('',(0.115470053837925,-0.5,-0.2));
#13435=CARTESIAN_POINT('',(0.23094010767585,-0.5,0.));
#13436=CARTESIAN_POINT('',(0.115470053837925,-0.8,-0.2));
#13437=CARTESIAN_POINT('',(0.115470053837925,-0.5,-0.2));
#13438=CARTESIAN_POINT('',(0.23094010767585,-0.8,0.));
#13439=CARTESIAN_POINT('',(0.23094010767585,-0.8,0.));
#13440=CARTESIAN_POINT('',(0.23094010767585,-0.5,0.));
#13441=CARTESIAN_POINT('Origin',(-0.115470053837925,-0.5,-0.2));
#13442=CARTESIAN_POINT('',(-0.115470053837925,-0.5,-0.2));
#13443=CARTESIAN_POINT('',(0.115470053837925,-0.5,-0.2));
#13444=CARTESIAN_POINT('',(-0.115470053837925,-0.8,-0.2));
#13445=CARTESIAN_POINT('',(-0.115470053837925,-0.5,-0.2));
#13446=CARTESIAN_POINT('',(0.115470053837925,-0.8,-0.2));
#13447=CARTESIAN_POINT('Origin',(-0.23094010767585,-0.5,-2.77555756156289E-17));
#13448=CARTESIAN_POINT('',(-0.23094010767585,-0.5,-2.82820063659975E-17));
#13449=CARTESIAN_POINT('',(-0.115470053837925,-0.5,-0.2));
#13450=CARTESIAN_POINT('',(-0.23094010767585,-0.8,-2.77555756156289E-17));
#13451=CARTESIAN_POINT('',(-0.23094010767585,-0.5,-2.82820063659975E-17));
#13452=CARTESIAN_POINT('',(-0.115470053837925,-0.8,-0.2));
#13453=CARTESIAN_POINT('Origin',(-0.115470053837925,-0.5,0.2));
#13454=CARTESIAN_POINT('',(-0.115470053837925,-0.5,0.2));
#13455=CARTESIAN_POINT('',(-0.23094010767585,-0.5,-2.82820063659975E-17));
#13456=CARTESIAN_POINT('',(-0.115470053837925,-0.8,0.2));
#13457=CARTESIAN_POINT('',(-0.115470053837925,-0.5,0.2));
#13458=CARTESIAN_POINT('',(-0.23094010767585,-0.8,-2.82820063659975E-17));
#13459=CARTESIAN_POINT('Origin',(0.115470053837925,-0.5,0.2));
#13460=CARTESIAN_POINT('',(0.115470053837925,-0.5,0.2));
#13461=CARTESIAN_POINT('',(-0.115470053837925,-0.5,0.2));
#13462=CARTESIAN_POINT('',(0.115470053837925,-0.8,0.2));
#13463=CARTESIAN_POINT('',(0.115470053837925,-0.5,0.2));
#13464=CARTESIAN_POINT('',(-0.115470053837925,-0.8,0.2));
#13465=CARTESIAN_POINT('Origin',(0.23094010767585,-0.5,0.));
#13466=CARTESIAN_POINT('',(0.115470053837925,-0.5,0.2));
#13467=CARTESIAN_POINT('',(0.115470053837925,-0.8,0.2));
#13468=CARTESIAN_POINT('Origin',(0.,-0.5,0.));
#13469=CARTESIAN_POINT('Origin',(0.,-0.8,0.));
#13470=CARTESIAN_POINT('Origin',(0.,-1.4,0.));
#13471=CARTESIAN_POINT('',(-0.24505,-1.4,3.00099698131059E-17));
#13472=CARTESIAN_POINT('Origin',(0.,-1.4,0.));
#13473=CARTESIAN_POINT('Origin',(0.375,0.5,0.));
#13474=CARTESIAN_POINT('',(-0.375,0.5,-4.59242549680257E-17));
#13475=CARTESIAN_POINT('Origin',(0.,0.5,0.));
#13476=CARTESIAN_POINT('Origin',(0.,0.475,0.));
#13477=CARTESIAN_POINT('',(-0.425,0.45,-5.20474889637625E-17));
#13478=CARTESIAN_POINT('Origin',(0.,0.45,0.));
#13479=CARTESIAN_POINT('',(-0.4,0.475,-4.89858719658941E-17));
#13480=CARTESIAN_POINT('Origin',(0.,0.24,0.));
#13481=CARTESIAN_POINT('',(-0.425,0.0299999999999998,-5.20474889637625E-17));
#13482=CARTESIAN_POINT('Origin',(0.,0.0299999999999998,0.));
#13483=CARTESIAN_POINT('',(-0.425,0.24,-5.20474889637625E-17));
#13484=CARTESIAN_POINT('Origin',(0.,0.0150000000000001,0.));
#13485=CARTESIAN_POINT('',(-0.395,4.85722573273506E-17,-4.83735485663204E-17));
#13486=CARTESIAN_POINT('Origin',(0.,0.,0.));
#13487=CARTESIAN_POINT('',(-0.41,0.0150000000000001,-5.02105187650415E-17));
#13488=CARTESIAN_POINT('Origin',(0.27,0.,0.));
#13489=CARTESIAN_POINT('',(-0.27,0.,-3.30654635769785E-17));
#13490=CARTESIAN_POINT('Origin',(0.,0.,0.));
#13491=CARTESIAN_POINT('Origin',(0.,-0.02,0.));
#13492=CARTESIAN_POINT('',(-0.24505,-0.0498999999999999,3.00099698131059E-17));
#13493=CARTESIAN_POINT('Origin',(0.,-0.0498999999999999,0.));
#13494=CARTESIAN_POINT('',(-0.26,-0.02,-3.18408167778312E-17));
#13495=CARTESIAN_POINT('Origin',(0.,-0.995,0.));
#13496=CARTESIAN_POINT('',(-0.24505,-0.995,-3.00099698131059E-17));
#13497=CARTESIAN_POINT('',(0.,0.,0.));
#13498=CARTESIAN_POINT('',(0.,0.,0.));
#13499=CARTESIAN_POINT('Origin',(0.,0.,0.));
#13500=CARTESIAN_POINT('',(-0.976185,-0.246528389340863,-1.19548183562566E-16));
#13501=CARTESIAN_POINT('',(-1.19548183562566E-16,-0.246528389340863,0.976185));
#13502=CARTESIAN_POINT('Origin',(0.,-0.246528389340863,0.));
#13503=CARTESIAN_POINT('Origin',(0.,-0.246528389340863,0.));
#13504=CARTESIAN_POINT('',(-1.19548183562566E-16,0.246528389340863,0.976185));
#13505=CARTESIAN_POINT('Origin',(-1.22464679914735E-16,0.,1.));
#13506=CARTESIAN_POINT('',(-0.976185,0.246528389340863,1.19548183562566E-16));
#13507=CARTESIAN_POINT('Origin',(0.,0.246528389340863,0.));
#13508=CARTESIAN_POINT('Origin',(0.,0.246528389340863,0.));
#13509=CARTESIAN_POINT('Origin',(0.,0.,0.));
#13510=CARTESIAN_POINT('',(-0.976185,0.45,-1.19548183562566E-16));
#13511=CARTESIAN_POINT('',(-0.976185,0.,-1.19548183562566E-16));
#13512=CARTESIAN_POINT('Origin',(0.,0.45,0.));
#13513=CARTESIAN_POINT('Origin',(0.,0.,0.));
#13514=CARTESIAN_POINT('',(-0.5,-0.39,-6.12323399573677E-17));
#13515=CARTESIAN_POINT('Origin',(0.,-0.39,0.));
#13516=CARTESIAN_POINT('',(-0.5,0.39,-6.12323399573677E-17));
#13517=CARTESIAN_POINT('',(-0.5,0.,-6.12323399573677E-17));
#13518=CARTESIAN_POINT('Origin',(0.,0.39,0.));
#13519=CARTESIAN_POINT('Origin',(0.,0.42,0.));
#13520=CARTESIAN_POINT('',(-0.56,0.45,-6.85802207522518E-17));
#13521=CARTESIAN_POINT('',(-0.53,0.42,-6.49062803548097E-17));
#13522=CARTESIAN_POINT('Origin',(0.,0.45,0.));
#13523=CARTESIAN_POINT('Origin',(0.976185,0.45,0.));
#13524=CARTESIAN_POINT('Origin',(0.,0.,0.));
#13525=CARTESIAN_POINT('',(-0.976185,-0.45,-1.19548183562566E-16));
#13526=CARTESIAN_POINT('Origin',(0.,-0.45,0.));
#13527=CARTESIAN_POINT('',(-0.976185,0.,-1.19548183562566E-16));
#13528=CARTESIAN_POINT('Origin',(0.56,-0.45,0.));
#13529=CARTESIAN_POINT('',(-0.56,-0.45,-6.85802207522518E-17));
#13530=CARTESIAN_POINT('Origin',(0.,-0.45,0.));
#13531=CARTESIAN_POINT('Origin',(0.,-0.42,0.));
#13532=CARTESIAN_POINT('',(-0.53,-0.42,-6.49062803548097E-17));
#13533=CARTESIAN_POINT('',(0.,0.,0.));
#13534=CARTESIAN_POINT('Origin',(0.,0.,0.));
#13535=CARTESIAN_POINT('',(-1.023815,0.246528389340863,-1.25381176266905E-16));
#13536=CARTESIAN_POINT('',(-1.25381176266905E-16,0.246528389340863,1.023815));
#13537=CARTESIAN_POINT('Origin',(0.,0.246528389340863,0.));
#13538=CARTESIAN_POINT('Origin',(0.,0.246528389340863,0.));
#13539=CARTESIAN_POINT('',(-1.25381176266905E-16,-0.246528389340863,1.023815));
#13540=CARTESIAN_POINT('Origin',(-1.22464679914735E-16,0.,1.));
#13541=CARTESIAN_POINT('',(-1.023815,-0.246528389340863,1.25381176266905E-16));
#13542=CARTESIAN_POINT('Origin',(0.,-0.246528389340863,0.));
#13543=CARTESIAN_POINT('Origin',(0.,-0.246528389340863,0.));
#13544=CARTESIAN_POINT('Origin',(0.,0.,0.));
#13545=CARTESIAN_POINT('',(-1.023815,-0.45,-1.25381176266905E-16));
#13546=CARTESIAN_POINT('Origin',(0.,-0.45,0.));
#13547=CARTESIAN_POINT('',(-1.023815,0.,-1.25381176266905E-16));
#13548=CARTESIAN_POINT('Origin',(1.44,0.45,0.));
#13549=CARTESIAN_POINT('',(-1.44,0.45,-1.76349139077219E-16));
#13550=CARTESIAN_POINT('Origin',(0.,0.45,0.));
#13551=CARTESIAN_POINT('',(-1.023815,0.45,-1.25381176266905E-16));
#13552=CARTESIAN_POINT('Origin',(0.,0.45,0.));
#13553=CARTESIAN_POINT('Origin',(0.,0.42,0.));
#13554=CARTESIAN_POINT('',(-1.5,0.39,-1.83697019872103E-16));
#13555=CARTESIAN_POINT('Origin',(0.,0.39,0.));
#13556=CARTESIAN_POINT('',(-1.47,0.42,-1.80023079474661E-16));
#13557=CARTESIAN_POINT('Origin',(0.,0.,0.));
#13558=CARTESIAN_POINT('',(-1.5,-0.39,-1.83697019872103E-16));
#13559=CARTESIAN_POINT('Origin',(0.,-0.39,0.));
#13560=CARTESIAN_POINT('',(-1.5,0.,-1.83697019872103E-16));
#13561=CARTESIAN_POINT('Origin',(0.,-0.42,0.));
#13562=CARTESIAN_POINT('',(-1.44,-0.45,-1.76349139077219E-16));
#13563=CARTESIAN_POINT('Origin',(0.,-0.45,0.));
#13564=CARTESIAN_POINT('',(-1.47,-0.42,-1.80023079474661E-16));
#13565=CARTESIAN_POINT('Origin',(1.023815,-0.45,0.));
#13566=CARTESIAN_POINT('Origin',(0.,0.,0.));
#13567=CARTESIAN_POINT('',(-1.023815,0.,-1.25381176266905E-16));
#13568=CARTESIAN_POINT('',(0.,0.,0.));
#13569=CARTESIAN_POINT('Origin',(1.,0.,0.));
#13570=CARTESIAN_POINT('',(1.,-1.78583896120461E-33,0.23815));
#13571=CARTESIAN_POINT('',(1.,-1.78583896120461E-33,-0.23815));
#13572=CARTESIAN_POINT('Origin',(1.,0.,0.));
#13573=CARTESIAN_POINT('Origin',(0.707106781186548,0.,-0.707106781186547));
#13574=CARTESIAN_POINT('',(0.875504261126124,-1.78583896120461E-33,-0.538709301246971));
#13575=CARTESIAN_POINT('',(0.538709301246971,-1.78583896120461E-33,-0.875504261126124));
#13576=CARTESIAN_POINT('Origin',(0.707106781186548,0.,-0.707106781186547));
#13577=CARTESIAN_POINT('Origin',(6.12323399573677E-17,0.,-1.));
#13578=CARTESIAN_POINT('',(0.23815,-1.78583896120461E-33,-1.));
#13579=CARTESIAN_POINT('',(-0.23815,-1.78583896120461E-33,-1.));
#13580=CARTESIAN_POINT('Origin',(6.12323399573677E-17,0.,-1.));
#13581=CARTESIAN_POINT('Origin',(-0.707106781186547,0.,-0.707106781186548));
#13582=CARTESIAN_POINT('',(-0.538709301246971,-1.78583896120461E-33,-0.875504261126124));
#13583=CARTESIAN_POINT('',(-0.875504261126124,-1.78583896120461E-33,-0.538709301246971));
#13584=CARTESIAN_POINT('Origin',(-0.707106781186547,0.,-0.707106781186548));
#13585=CARTESIAN_POINT('Origin',(-1.,0.,-1.22464679914735E-16));
#13586=CARTESIAN_POINT('',(-1.,-1.78583896120461E-33,-0.23815));
#13587=CARTESIAN_POINT('',(-1.,-1.78583896120461E-33,0.23815));
#13588=CARTESIAN_POINT('Origin',(-1.,0.,-1.22464679914735E-16));
#13589=CARTESIAN_POINT('Origin',(-0.707106781186548,0.,0.707106781186547));
#13590=CARTESIAN_POINT('',(-0.875504261126124,-7.94881478324376E-33,0.538709301246971));
#13591=CARTESIAN_POINT('',(-0.538709301246971,4.37713686083455E-33,0.875504261126124));
#13592=CARTESIAN_POINT('Origin',(-0.707106781186548,0.,0.707106781186547));
#13593=CARTESIAN_POINT('Origin',(-1.83697019872103E-16,0.,1.));
#13594=CARTESIAN_POINT('',(-0.23815,-1.78583896120461E-33,1.));
#13595=CARTESIAN_POINT('',(0.23815,-1.78583896120461E-33,1.));
#13596=CARTESIAN_POINT('Origin',(-1.83697019872103E-16,0.,1.));
#13597=CARTESIAN_POINT('Origin',(0.707106781186547,0.,0.707106781186548));
#13598=CARTESIAN_POINT('',(0.538709301246971,-4.86732687222419E-33,0.875504261126124));
#13599=CARTESIAN_POINT('',(0.875504261126124,1.29564894981497E-33,0.538709301246971));
#13600=CARTESIAN_POINT('Origin',(0.707106781186547,0.,0.707106781186548));
#13601=CARTESIAN_POINT('',(0.,0.,0.));
#13602=CARTESIAN_POINT('Origin',(0.707106781186547,0.,0.707106781186548));
#13603=CARTESIAN_POINT('',(0.504455939115715,-0.04763,0.841298510752802));
#13604=CARTESIAN_POINT('',(0.841298510752802,-0.04763,0.504455939115715));
#13605=CARTESIAN_POINT('Ctrl Pts',(0.504455939115715,-0.04763,0.841298510752802));
#13606=CARTESIAN_POINT('Ctrl Pts',(0.508899795931835,-0.0740444353928835,
0.838633903678357));
#13607=CARTESIAN_POINT('Ctrl Pts',(0.517157748491652,-0.0999305678883309,
0.833661031856294));
#13608=CARTESIAN_POINT('Ctrl Pts',(0.537715343527944,-0.142345102874864,
0.820511285096538));
#13609=CARTESIAN_POINT('Ctrl Pts',(0.548874290046456,-0.159766064500479,
0.813159949759));
#13610=CARTESIAN_POINT('Ctrl Pts',(0.573915184558107,-0.190326085855194,
0.795684265985089));
#13611=CARTESIAN_POINT('Ctrl Pts',(0.587792702767295,-0.203463743702801,
0.78555112003688));
#13612=CARTESIAN_POINT('Ctrl Pts',(0.615966552324775,-0.224161999508995,
0.763642258217233));
#13613=CARTESIAN_POINT('Ctrl Pts',(0.631684198665438,-0.232861760990032,
0.750785745543687));
#13614=CARTESIAN_POINT('Ctrl Pts',(0.663382628119203,-0.244251601209411,
0.722929908501543));
#13615=CARTESIAN_POINT('Ctrl Pts',(0.679352081686668,-0.246942143572133,
0.707917883896095));
#13616=CARTESIAN_POINT('Ctrl Pts',(0.707917883896095,-0.246942143572133,
0.679352081686668));
#13617=CARTESIAN_POINT('Ctrl Pts',(0.722929908501543,-0.244251601209411,
0.663382628119203));
#13618=CARTESIAN_POINT('Ctrl Pts',(0.750785745543687,-0.232861760990032,
0.631684198665439));
#13619=CARTESIAN_POINT('Ctrl Pts',(0.763642258217232,-0.224161999508995,
0.615966552324775));
#13620=CARTESIAN_POINT('Ctrl Pts',(0.78555112003688,-0.203463743702801,
0.587792702767295));
#13621=CARTESIAN_POINT('Ctrl Pts',(0.795684265985088,-0.190326085855194,
0.573915184558108));
#13622=CARTESIAN_POINT('Ctrl Pts',(0.813159949759,-0.15976606450048,0.548874290046456));
#13623=CARTESIAN_POINT('Ctrl Pts',(0.820511285096538,-0.142345102874864,
0.537715343527944));
#13624=CARTESIAN_POINT('Ctrl Pts',(0.833661031856294,-0.099930567888331,
0.517157748491653));
#13625=CARTESIAN_POINT('Ctrl Pts',(0.838633903678357,-0.0740444353928835,
0.508899795931835));
#13626=CARTESIAN_POINT('Ctrl Pts',(0.841298510752801,-0.0476299999999999,
0.504455939115715));
#13627=CARTESIAN_POINT('',(0.528110872004958,-0.04763,0.871530771444223));
#13628=CARTESIAN_POINT('Origin',(0.707106781186547,-0.04763,0.707106781186548));
#13629=CARTESIAN_POINT('',(0.871530771444223,-0.04763,0.528110872004959));
#13630=CARTESIAN_POINT('Ctrl Pts',(0.871530771444223,-0.0476300000000001,
0.528110872004958));
#13631=CARTESIAN_POINT('Ctrl Pts',(0.87014664509073,-0.0609922781173483,
0.530395067942936));
#13632=CARTESIAN_POINT('Ctrl Pts',(0.868149331745851,-0.0742967091364493,
0.533674141594226));
#13633=CARTESIAN_POINT('Ctrl Pts',(0.85981294420286,-0.115492077056649,
0.54708917182331));
#13634=CARTESIAN_POINT('Ctrl Pts',(0.850993704737257,-0.141695629206859,
0.560922177770136));
#13635=CARTESIAN_POINT('Ctrl Pts',(0.830754510485543,-0.181890537957859,
0.590422647829571));
#13636=CARTESIAN_POINT('Ctrl Pts',(0.816896541396381,-0.201072148666545,
0.609616703125488));
#13637=CARTESIAN_POINT('Ctrl Pts',(0.792310597819928,-0.223955109275652,
0.641117951819998));
#13638=CARTESIAN_POINT('Ctrl Pts',(0.779109323683612,-0.232742381310829,
0.657208095763053));
#13639=CARTESIAN_POINT('Ctrl Pts',(0.750552691816206,-0.244234834628584,
0.68964083160521));
#13640=CARTESIAN_POINT('Ctrl Pts',(0.735185187071673,-0.246942143572133,
0.705971972091755));
#13641=CARTESIAN_POINT('Ctrl Pts',(0.705971972091754,-0.246942143572133,
0.735185187071673));
#13642=CARTESIAN_POINT('Ctrl Pts',(0.689640831605209,-0.244234834628584,
0.750552691816206));
#13643=CARTESIAN_POINT('Ctrl Pts',(0.657208095763052,-0.232742381310829,
0.779109323683612));
#13644=CARTESIAN_POINT('Ctrl Pts',(0.641117951819998,-0.223955109275652,
0.792310597819928));
#13645=CARTESIAN_POINT('Ctrl Pts',(0.609616703125487,-0.201072148666545,
0.816896541396382));
#13646=CARTESIAN_POINT('Ctrl Pts',(0.590422647829571,-0.181890537957858,
0.830754510485544));
#13647=CARTESIAN_POINT('Ctrl Pts',(0.560922177770135,-0.141695629206858,
0.850993704737257));
#13648=CARTESIAN_POINT('Ctrl Pts',(0.547089171823309,-0.115492077056649,
0.859812944202861));
#13649=CARTESIAN_POINT('Ctrl Pts',(0.533674141594226,-0.0742967091364491,
0.868149331745852));
#13650=CARTESIAN_POINT('Ctrl Pts',(0.530395067942936,-0.0609922781173483,
0.870146645090731));
#13651=CARTESIAN_POINT('Ctrl Pts',(0.528110872004958,-0.0476300000000001,
0.871530771444223));
#13652=CARTESIAN_POINT('Origin',(0.707106781186547,-0.04763,0.707106781186548));
#13653=CARTESIAN_POINT('Origin',(0.,-0.166705,0.));
#13654=CARTESIAN_POINT('',(0.242834539687906,-0.04763,0.989696097314));
#13655=CARTESIAN_POINT('Origin',(0.,-0.04763,0.));
#13656=CARTESIAN_POINT('',(-0.242834539687907,-0.04763,0.989696097314));
#13657=CARTESIAN_POINT('Ctrl Pts',(0.242834539687906,-0.04763,0.989696097314));
#13658=CARTESIAN_POINT('Ctrl Pts',(0.24024064412003,-0.0609922781173483,
0.990332542620729));
#13659=CARTESIAN_POINT('Ctrl Pts',(0.236509675094874,-0.0742967091364492,
0.991238884025248));
#13660=CARTESIAN_POINT('Ctrl Pts',(0.221129100087819,-0.115492077056649,
0.994830026707808));
#13661=CARTESIAN_POINT('Ctrl Pts',(0.205111543747588,-0.141695629206859,
0.998375294985966));
#13662=CARTESIAN_POINT('Ctrl Pts',(0.169940289819232,-0.181890537957859,
1.00492400591205));
#13663=CARTESIAN_POINT('Ctrl Pts',(0.1465689792446,-0.201072148666545,1.00869718865384));
#13664=CARTESIAN_POINT('Ctrl Pts',(0.106909345252087,-0.223955109275652,
1.01358704779679));
#13665=CARTESIAN_POINT('Ctrl Pts',(0.0861971848975941,-0.232742381310829,
1.0156297872271));
#13666=CARTESIAN_POINT('Ctrl Pts',(0.0430711894098822,-0.244234834628584,
1.01837060663223));
#13667=CARTESIAN_POINT('Ctrl Pts',(0.0206568624125605,-0.246942143572133,
1.019052));
#13668=CARTESIAN_POINT('Ctrl Pts',(-0.0206568624125608,-0.246942143572133,
1.019052));
#13669=CARTESIAN_POINT('Ctrl Pts',(-0.0430711894098825,-0.244234834628584,
1.01837060663223));
#13670=CARTESIAN_POINT('Ctrl Pts',(-0.0861971848975943,-0.232742381310829,
1.0156297872271));
#13671=CARTESIAN_POINT('Ctrl Pts',(-0.106909345252088,-0.223955109275652,
1.01358704779679));
#13672=CARTESIAN_POINT('Ctrl Pts',(-0.1465689792446,-0.201072148666545,
1.00869718865384));
#13673=CARTESIAN_POINT('Ctrl Pts',(-0.169940289819232,-0.181890537957859,
1.00492400591205));
#13674=CARTESIAN_POINT('Ctrl Pts',(-0.205111543747588,-0.141695629206859,
0.998375294985966));
#13675=CARTESIAN_POINT('Ctrl Pts',(-0.221129100087819,-0.115492077056649,
0.994830026707808));
#13676=CARTESIAN_POINT('Ctrl Pts',(-0.236509675094875,-0.0742967091364493,
0.991238884025248));
#13677=CARTESIAN_POINT('Ctrl Pts',(-0.24024064412003,-0.0609922781173483,
0.990332542620729));
#13678=CARTESIAN_POINT('Ctrl Pts',(-0.242834539687907,-0.04763,0.989696097314));
#13679=CARTESIAN_POINT('',(-0.528110872004959,-0.04763,0.871530771444223));
#13680=CARTESIAN_POINT('Origin',(0.,-0.04763,0.));
#13681=CARTESIAN_POINT('',(-0.871530771444223,-0.04763,0.528110872004958));
#13682=CARTESIAN_POINT('Ctrl Pts',(-0.528110872004958,-0.0476300000000001,
0.871530771444223));
#13683=CARTESIAN_POINT('Ctrl Pts',(-0.530395067942936,-0.0609922781173484,
0.87014664509073));
#13684=CARTESIAN_POINT('Ctrl Pts',(-0.533674141594226,-0.0742967091364493,
0.868149331745851));
#13685=CARTESIAN_POINT('Ctrl Pts',(-0.54708917182331,-0.115492077056649,
0.85981294420286));
#13686=CARTESIAN_POINT('Ctrl Pts',(-0.560922177770136,-0.141695629206859,
0.850993704737257));
#13687=CARTESIAN_POINT('Ctrl Pts',(-0.590422647829571,-0.181890537957859,
0.830754510485543));
#13688=CARTESIAN_POINT('Ctrl Pts',(-0.609616703125488,-0.201072148666545,
0.816896541396381));
#13689=CARTESIAN_POINT('Ctrl Pts',(-0.641117951819998,-0.223955109275652,
0.792310597819928));
#13690=CARTESIAN_POINT('Ctrl Pts',(-0.657208095763053,-0.232742381310829,
0.779109323683611));
#13691=CARTESIAN_POINT('Ctrl Pts',(-0.68964083160521,-0.244234834628584,
0.750552691816205));
#13692=CARTESIAN_POINT('Ctrl Pts',(-0.705971972091755,-0.246942143572133,
0.735185187071673));
#13693=CARTESIAN_POINT('Ctrl Pts',(-0.735185187071673,-0.246942143572133,
0.705971972091754));
#13694=CARTESIAN_POINT('Ctrl Pts',(-0.750552691816206,-0.244234834628584,
0.689640831605209));
#13695=CARTESIAN_POINT('Ctrl Pts',(-0.779109323683612,-0.232742381310829,
0.657208095763052));
#13696=CARTESIAN_POINT('Ctrl Pts',(-0.792310597819928,-0.223955109275652,
0.641117951819998));
#13697=CARTESIAN_POINT('Ctrl Pts',(-0.816896541396382,-0.201072148666545,
0.609616703125487));
#13698=CARTESIAN_POINT('Ctrl Pts',(-0.830754510485544,-0.181890537957858,
0.590422647829571));
#13699=CARTESIAN_POINT('Ctrl Pts',(-0.850993704737257,-0.141695629206858,
0.560922177770135));
#13700=CARTESIAN_POINT('Ctrl Pts',(-0.859812944202861,-0.115492077056649,
0.547089171823309));
#13701=CARTESIAN_POINT('Ctrl Pts',(-0.868149331745852,-0.0742967091364491,
0.533674141594226));
#13702=CARTESIAN_POINT('Ctrl Pts',(-0.870146645090731,-0.0609922781173483,
0.530395067942936));
#13703=CARTESIAN_POINT('Ctrl Pts',(-0.871530771444223,-0.04763,0.528110872004958));
#13704=CARTESIAN_POINT('',(-0.989696097314,-0.04763,0.242834539687906));
#13705=CARTESIAN_POINT('Origin',(0.,-0.04763,0.));
#13706=CARTESIAN_POINT('',(-1.019052,-0.246942143572133,1.248489836334E-16));
#13707=CARTESIAN_POINT('Ctrl Pts',(-0.989696097314,-0.04763,0.242834539687906));
#13708=CARTESIAN_POINT('Ctrl Pts',(-0.990332542620729,-0.0609922781173483,
0.24024064412003));
#13709=CARTESIAN_POINT('Ctrl Pts',(-0.991238884025248,-0.0742967091364492,
0.236509675094874));
#13710=CARTESIAN_POINT('Ctrl Pts',(-0.994830026707808,-0.115492077056649,
0.221129100087819));
#13711=CARTESIAN_POINT('Ctrl Pts',(-0.998375294985966,-0.141695629206859,
0.205111543747588));
#13712=CARTESIAN_POINT('Ctrl Pts',(-1.00492400591205,-0.181890537957859,
0.169940289819232));
#13713=CARTESIAN_POINT('Ctrl Pts',(-1.00869718865384,-0.201072148666545,
0.1465689792446));
#13714=CARTESIAN_POINT('Ctrl Pts',(-1.01358704779679,-0.223955109275652,
0.106909345252088));
#13715=CARTESIAN_POINT('Ctrl Pts',(-1.0156297872271,-0.232742381310829,
0.0861971848975944));
#13716=CARTESIAN_POINT('Ctrl Pts',(-1.01837060663223,-0.244234834628584,
0.0430711894098825));
#13717=CARTESIAN_POINT('Ctrl Pts',(-1.019052,-0.246942143572133,0.0206568624125608));
#13718=CARTESIAN_POINT('Ctrl Pts',(-1.019052,-0.246942143572133,1.2490009027033E-16));
#13719=CARTESIAN_POINT('',(-1.019052,-0.28578,1.24797876996471E-16));
#13720=CARTESIAN_POINT('',(-1.019052,-0.166705,1.24797876996471E-16));
#13721=CARTESIAN_POINT('Origin',(0.,-0.28578,0.));
#13722=CARTESIAN_POINT('',(-0.989696097314,-0.04763,-0.242834539687906));
#13723=CARTESIAN_POINT('Ctrl Pts',(-1.019052,-0.246942143572133,1.2490009027033E-16));
#13724=CARTESIAN_POINT('Ctrl Pts',(-1.019052,-0.246942143572133,-0.0206568624125605));
#13725=CARTESIAN_POINT('Ctrl Pts',(-1.01837060663223,-0.244234834628584,
-0.0430711894098822));
#13726=CARTESIAN_POINT('Ctrl Pts',(-1.0156297872271,-0.232742381310829,
-0.0861971848975941));
#13727=CARTESIAN_POINT('Ctrl Pts',(-1.01358704779679,-0.223955109275652,
-0.106909345252087));
#13728=CARTESIAN_POINT('Ctrl Pts',(-1.00869718865384,-0.201072148666546,
-0.1465689792446));
#13729=CARTESIAN_POINT('Ctrl Pts',(-1.00492400591205,-0.181890537957859,
-0.169940289819232));
#13730=CARTESIAN_POINT('Ctrl Pts',(-0.998375294985966,-0.141695629206859,
-0.205111543747588));
#13731=CARTESIAN_POINT('Ctrl Pts',(-0.994830026707808,-0.11549207705665,
-0.221129100087819));
#13732=CARTESIAN_POINT('Ctrl Pts',(-0.991238884025248,-0.0742967091364495,
-0.236509675094874));
#13733=CARTESIAN_POINT('Ctrl Pts',(-0.990332542620729,-0.0609922781173484,
-0.24024064412003));
#13734=CARTESIAN_POINT('Ctrl Pts',(-0.989696097314,-0.0476300000000001,
-0.242834539687907));
#13735=CARTESIAN_POINT('',(-0.871530771444223,-0.04763,-0.528110872004958));
#13736=CARTESIAN_POINT('Origin',(0.,-0.04763,0.));
#13737=CARTESIAN_POINT('',(-0.528110872004958,-0.04763,-0.871530771444223));
#13738=CARTESIAN_POINT('Ctrl Pts',(-0.871530771444223,-0.0476300000000001,
-0.528110872004958));
#13739=CARTESIAN_POINT('Ctrl Pts',(-0.87014664509073,-0.0609922781173484,
-0.530395067942936));
#13740=CARTESIAN_POINT('Ctrl Pts',(-0.868149331745851,-0.0742967091364494,
-0.533674141594226));
#13741=CARTESIAN_POINT('Ctrl Pts',(-0.85981294420286,-0.115492077056649,
-0.54708917182331));
#13742=CARTESIAN_POINT('Ctrl Pts',(-0.850993704737257,-0.141695629206859,
-0.560922177770136));
#13743=CARTESIAN_POINT('Ctrl Pts',(-0.830754510485543,-0.181890537957859,
-0.590422647829571));
#13744=CARTESIAN_POINT('Ctrl Pts',(-0.816896541396381,-0.201072148666546,
-0.609616703125488));
#13745=CARTESIAN_POINT('Ctrl Pts',(-0.792310597819928,-0.223955109275652,
-0.641117951819999));
#13746=CARTESIAN_POINT('Ctrl Pts',(-0.779109323683611,-0.232742381310829,
-0.657208095763053));
#13747=CARTESIAN_POINT('Ctrl Pts',(-0.750552691816205,-0.244234834628584,
-0.68964083160521));
#13748=CARTESIAN_POINT('Ctrl Pts',(-0.735185187071673,-0.246942143572133,
-0.705971972091755));
#13749=CARTESIAN_POINT('Ctrl Pts',(-0.705971972091754,-0.246942143572133,
-0.735185187071673));
#13750=CARTESIAN_POINT('Ctrl Pts',(-0.68964083160521,-0.244234834628584,
-0.750552691816206));
#13751=CARTESIAN_POINT('Ctrl Pts',(-0.657208095763052,-0.232742381310829,
-0.779109323683612));
#13752=CARTESIAN_POINT('Ctrl Pts',(-0.641117951819998,-0.223955109275652,
-0.792310597819928));
#13753=CARTESIAN_POINT('Ctrl Pts',(-0.609616703125488,-0.201072148666545,
-0.816896541396381));
#13754=CARTESIAN_POINT('Ctrl Pts',(-0.590422647829571,-0.181890537957859,
-0.830754510485543));
#13755=CARTESIAN_POINT('Ctrl Pts',(-0.560922177770136,-0.141695629206859,
-0.850993704737257));
#13756=CARTESIAN_POINT('Ctrl Pts',(-0.54708917182331,-0.115492077056649,
-0.85981294420286));
#13757=CARTESIAN_POINT('Ctrl Pts',(-0.533674141594226,-0.0742967091364494,
-0.868149331745852));
#13758=CARTESIAN_POINT('Ctrl Pts',(-0.530395067942936,-0.0609922781173484,
-0.870146645090731));
#13759=CARTESIAN_POINT('Ctrl Pts',(-0.528110872004958,-0.0476300000000001,
-0.871530771444223));
#13760=CARTESIAN_POINT('',(-0.242834539687906,-0.04763,-0.989696097314));
#13761=CARTESIAN_POINT('Origin',(0.,-0.04763,0.));
#13762=CARTESIAN_POINT('',(0.242834539687906,-0.04763,-0.989696097314));
#13763=CARTESIAN_POINT('Ctrl Pts',(-0.242834539687907,-0.04763,-0.989696097314));
#13764=CARTESIAN_POINT('Ctrl Pts',(-0.24024064412003,-0.0609922781173483,
-0.990332542620729));
#13765=CARTESIAN_POINT('Ctrl Pts',(-0.236509675094874,-0.0742967091364493,
-0.991238884025248));
#13766=CARTESIAN_POINT('Ctrl Pts',(-0.221129100087819,-0.115492077056649,
-0.994830026707808));
#13767=CARTESIAN_POINT('Ctrl Pts',(-0.205111543747588,-0.141695629206859,
-0.998375294985966));
#13768=CARTESIAN_POINT('Ctrl Pts',(-0.169940289819232,-0.181890537957859,
-1.00492400591205));
#13769=CARTESIAN_POINT('Ctrl Pts',(-0.1465689792446,-0.201072148666545,
-1.00869718865384));
#13770=CARTESIAN_POINT('Ctrl Pts',(-0.106909345252087,-0.223955109275652,
-1.01358704779679));
#13771=CARTESIAN_POINT('Ctrl Pts',(-0.0861971848975942,-0.232742381310829,
-1.0156297872271));
#13772=CARTESIAN_POINT('Ctrl Pts',(-0.0430711894098823,-0.244234834628584,
-1.01837060663223));
#13773=CARTESIAN_POINT('Ctrl Pts',(-0.0206568624125606,-0.246942143572133,
-1.019052));
#13774=CARTESIAN_POINT('Ctrl Pts',(0.0206568624125607,-0.246942143572133,
-1.019052));
#13775=CARTESIAN_POINT('Ctrl Pts',(0.0430711894098824,-0.244234834628584,
-1.01837060663223));
#13776=CARTESIAN_POINT('Ctrl Pts',(0.0861971848975943,-0.232742381310829,
-1.0156297872271));
#13777=CARTESIAN_POINT('Ctrl Pts',(0.106909345252088,-0.223955109275652,
-1.01358704779679));
#13778=CARTESIAN_POINT('Ctrl Pts',(0.1465689792446,-0.201072148666545,-1.00869718865384));
#13779=CARTESIAN_POINT('Ctrl Pts',(0.169940289819232,-0.181890537957859,
-1.00492400591205));
#13780=CARTESIAN_POINT('Ctrl Pts',(0.205111543747588,-0.141695629206859,
-0.998375294985966));
#13781=CARTESIAN_POINT('Ctrl Pts',(0.221129100087819,-0.115492077056649,
-0.994830026707808));
#13782=CARTESIAN_POINT('Ctrl Pts',(0.236509675094874,-0.0742967091364493,
-0.991238884025248));
#13783=CARTESIAN_POINT('Ctrl Pts',(0.24024064412003,-0.0609922781173484,
-0.990332542620729));
#13784=CARTESIAN_POINT('Ctrl Pts',(0.242834539687907,-0.04763,-0.989696097314));
#13785=CARTESIAN_POINT('',(0.528110872004958,-0.04763,-0.871530771444223));
#13786=CARTESIAN_POINT('Origin',(0.,-0.04763,0.));
#13787=CARTESIAN_POINT('',(0.871530771444223,-0.04763,-0.528110872004958));
#13788=CARTESIAN_POINT('Ctrl Pts',(0.528110872004958,-0.0476300000000001,
-0.871530771444223));
#13789=CARTESIAN_POINT('Ctrl Pts',(0.530395067942936,-0.0609922781173484,
-0.870146645090731));
#13790=CARTESIAN_POINT('Ctrl Pts',(0.533674141594226,-0.0742967091364493,
-0.868149331745851));
#13791=CARTESIAN_POINT('Ctrl Pts',(0.54708917182331,-0.115492077056649,
-0.85981294420286));
#13792=CARTESIAN_POINT('Ctrl Pts',(0.560922177770136,-0.141695629206859,
-0.850993704737257));
#13793=CARTESIAN_POINT('Ctrl Pts',(0.590422647829571,-0.181890537957859,
-0.830754510485543));
#13794=CARTESIAN_POINT('Ctrl Pts',(0.609616703125488,-0.201072148666545,
-0.816896541396381));
#13795=CARTESIAN_POINT('Ctrl Pts',(0.641117951819998,-0.223955109275652,
-0.792310597819928));
#13796=CARTESIAN_POINT('Ctrl Pts',(0.657208095763053,-0.232742381310829,
-0.779109323683612));
#13797=CARTESIAN_POINT('Ctrl Pts',(0.68964083160521,-0.244234834628584,
-0.750552691816206));
#13798=CARTESIAN_POINT('Ctrl Pts',(0.705971972091755,-0.246942143572133,
-0.735185187071673));
#13799=CARTESIAN_POINT('Ctrl Pts',(0.735185187071673,-0.246942143572133,
-0.705971972091754));
#13800=CARTESIAN_POINT('Ctrl Pts',(0.750552691816206,-0.244234834628584,
-0.68964083160521));
#13801=CARTESIAN_POINT('Ctrl Pts',(0.779109323683612,-0.232742381310829,
-0.657208095763053));
#13802=CARTESIAN_POINT('Ctrl Pts',(0.792310597819928,-0.223955109275652,
-0.641117951819998));
#13803=CARTESIAN_POINT('Ctrl Pts',(0.816896541396381,-0.201072148666545,
-0.609616703125488));
#13804=CARTESIAN_POINT('Ctrl Pts',(0.830754510485543,-0.181890537957859,
-0.590422647829571));
#13805=CARTESIAN_POINT('Ctrl Pts',(0.850993704737257,-0.141695629206859,
-0.560922177770136));
#13806=CARTESIAN_POINT('Ctrl Pts',(0.85981294420286,-0.115492077056649,
-0.54708917182331));
#13807=CARTESIAN_POINT('Ctrl Pts',(0.868149331745851,-0.0742967091364493,
-0.533674141594226));
#13808=CARTESIAN_POINT('Ctrl Pts',(0.870146645090731,-0.0609922781173484,
-0.530395067942936));
#13809=CARTESIAN_POINT('Ctrl Pts',(0.871530771444223,-0.0476300000000001,
-0.528110872004958));
#13810=CARTESIAN_POINT('',(0.989696097314,-0.04763,-0.242834539687906));
#13811=CARTESIAN_POINT('Origin',(0.,-0.04763,0.));
#13812=CARTESIAN_POINT('',(0.989696097314,-0.04763,0.242834539687906));
#13813=CARTESIAN_POINT('Ctrl Pts',(0.989696097314,-0.04763,-0.242834539687907));
#13814=CARTESIAN_POINT('Ctrl Pts',(0.990332542620729,-0.0609922781173483,
-0.24024064412003));
#13815=CARTESIAN_POINT('Ctrl Pts',(0.991238884025248,-0.0742967091364493,
-0.236509675094874));
#13816=CARTESIAN_POINT('Ctrl Pts',(0.994830026707808,-0.115492077056649,
-0.221129100087819));
#13817=CARTESIAN_POINT('Ctrl Pts',(0.998375294985966,-0.141695629206859,
-0.205111543747588));
#13818=CARTESIAN_POINT('Ctrl Pts',(1.00492400591205,-0.181890537957859,
-0.169940289819232));
#13819=CARTESIAN_POINT('Ctrl Pts',(1.00869718865384,-0.201072148666545,
-0.1465689792446));
#13820=CARTESIAN_POINT('Ctrl Pts',(1.01358704779679,-0.223955109275652,
-0.106909345252087));
#13821=CARTESIAN_POINT('Ctrl Pts',(1.0156297872271,-0.232742381310829,-0.0861971848975942));
#13822=CARTESIAN_POINT('Ctrl Pts',(1.01837060663223,-0.244234834628584,
-0.0430711894098823));
#13823=CARTESIAN_POINT('Ctrl Pts',(1.019052,-0.246942143572133,-0.0206568624125607));
#13824=CARTESIAN_POINT('Ctrl Pts',(1.019052,-0.246942143572133,0.0206568624125607));
#13825=CARTESIAN_POINT('Ctrl Pts',(1.01837060663223,-0.244234834628584,
0.0430711894098823));
#13826=CARTESIAN_POINT('Ctrl Pts',(1.0156297872271,-0.232742381310829,0.0861971848975942));
#13827=CARTESIAN_POINT('Ctrl Pts',(1.01358704779679,-0.223955109275652,
0.106909345252087));
#13828=CARTESIAN_POINT('Ctrl Pts',(1.00869718865384,-0.201072148666545,
0.1465689792446));
#13829=CARTESIAN_POINT('Ctrl Pts',(1.00492400591205,-0.181890537957859,
0.169940289819232));
#13830=CARTESIAN_POINT('Ctrl Pts',(0.998375294985966,-0.141695629206859,
0.205111543747588));
#13831=CARTESIAN_POINT('Ctrl Pts',(0.994830026707808,-0.115492077056649,
0.221129100087819));
#13832=CARTESIAN_POINT('Ctrl Pts',(0.991238884025248,-0.0742967091364492,
0.236509675094874));
#13833=CARTESIAN_POINT('Ctrl Pts',(0.990332542620729,-0.0609922781173483,
0.24024064412003));
#13834=CARTESIAN_POINT('Ctrl Pts',(0.989696097314,-0.04763,0.242834539687907));
#13835=CARTESIAN_POINT('Origin',(0.,-0.04763,0.));
#13836=CARTESIAN_POINT('Origin',(0.,-0.04763,0.));
#13837=CARTESIAN_POINT('',(0.238183666596899,-0.04763,0.951592097314));
#13838=CARTESIAN_POINT('Origin',(0.,-0.04763,0.));
#13839=CARTESIAN_POINT('Origin',(-1.94289029309402E-16,-0.04763,1.));
#13840=CARTESIAN_POINT('Origin',(-1.94289029309402E-16,0.,1.));
#13841=CARTESIAN_POINT('',(-0.2381836665969,-0.04763,0.951592097314));
#13842=CARTESIAN_POINT('Ctrl Pts',(-0.238183666596899,-0.0476299999999999,
0.951592097314));
#13843=CARTESIAN_POINT('Ctrl Pts',(-0.233157223576062,-0.0740444353928835,
0.952850216871763));
#13844=CARTESIAN_POINT('Ctrl Pts',(-0.223801617934946,-0.0999305678883309,
0.955173119738174));
#13845=CARTESIAN_POINT('Ctrl Pts',(-0.199966927975188,-0.142345102874864,
0.960411259488514));
#13846=CARTESIAN_POINT('Ctrl Pts',(-0.1868781821531,-0.159766064500479,
0.963103647174702));
#13847=CARTESIAN_POINT('Ctrl Pts',(-0.15681442133453,-0.190326085855194,
0.968453058988463));
#13848=CARTESIAN_POINT('Ctrl Pts',(-0.139836317888043,-0.203463743702801,
0.971100730005489));
#13849=CARTESIAN_POINT('Ctrl Pts',(-0.104422493053067,-0.224161999508995,
0.975530745318961));
#13850=CARTESIAN_POINT('Ctrl Pts',(-0.0842175114474176,-0.232861760990032,
0.977553872336861));
#13851=CARTESIAN_POINT('Ctrl Pts',(-0.0421062857595701,-0.244251601209411,
0.980270995488453));
#13852=CARTESIAN_POINT('Ctrl Pts',(-0.0201990724523197,-0.246942143572133,
0.980948));
#13853=CARTESIAN_POINT('Ctrl Pts',(0.020199072452319,-0.246942143572133,
0.980948));
#13854=CARTESIAN_POINT('Ctrl Pts',(0.0421062857595694,-0.244251601209411,
0.980270995488454));
#13855=CARTESIAN_POINT('Ctrl Pts',(0.0842175114474169,-0.232861760990032,
0.977553872336861));
#13856=CARTESIAN_POINT('Ctrl Pts',(0.104422493053067,-0.224161999508995,
0.975530745318961));
#13857=CARTESIAN_POINT('Ctrl Pts',(0.139836317888042,-0.203463743702801,
0.971100730005489));
#13858=CARTESIAN_POINT('Ctrl Pts',(0.15681442133453,-0.190326085855194,
0.968453058988463));
#13859=CARTESIAN_POINT('Ctrl Pts',(0.1868781821531,-0.15976606450048,0.963103647174702));
#13860=CARTESIAN_POINT('Ctrl Pts',(0.199966927975188,-0.142345102874864,
0.960411259488514));
#13861=CARTESIAN_POINT('Ctrl Pts',(0.223801617934945,-0.0999305678883309,
0.955173119738174));
#13862=CARTESIAN_POINT('Ctrl Pts',(0.233157223576061,-0.0740444353928835,
0.952850216871763));
#13863=CARTESIAN_POINT('Ctrl Pts',(0.238183666596899,-0.0476299999999999,
0.951592097314));
#13864=CARTESIAN_POINT('Origin',(-1.94289029309402E-16,-0.04763,1.));
#13865=CARTESIAN_POINT('Origin',(0.,-0.04763,0.));
#13866=CARTESIAN_POINT('',(-0.504455939115715,-0.04763,0.841298510752802));
#13867=CARTESIAN_POINT('Origin',(0.,-0.04763,0.));
#13868=CARTESIAN_POINT('Origin',(-0.707106781186548,-0.04763,0.707106781186547));
#13869=CARTESIAN_POINT('Origin',(-0.707106781186548,0.,0.707106781186547));
#13870=CARTESIAN_POINT('',(-0.841298510752802,-0.04763,0.504455939115715));
#13871=CARTESIAN_POINT('Ctrl Pts',(-0.841298510752802,-0.04763,0.504455939115715));
#13872=CARTESIAN_POINT('Ctrl Pts',(-0.838633903678357,-0.0740444353928835,
0.508899795931835));
#13873=CARTESIAN_POINT('Ctrl Pts',(-0.833661031856294,-0.0999305678883309,
0.517157748491652));
#13874=CARTESIAN_POINT('Ctrl Pts',(-0.820511285096538,-0.142345102874864,
0.537715343527944));
#13875=CARTESIAN_POINT('Ctrl Pts',(-0.813159949759,-0.159766064500479,0.548874290046456));
#13876=CARTESIAN_POINT('Ctrl Pts',(-0.795684265985089,-0.190326085855194,
0.573915184558107));
#13877=CARTESIAN_POINT('Ctrl Pts',(-0.78555112003688,-0.203463743702801,
0.587792702767295));
#13878=CARTESIAN_POINT('Ctrl Pts',(-0.763642258217233,-0.224161999508995,
0.615966552324775));
#13879=CARTESIAN_POINT('Ctrl Pts',(-0.750785745543687,-0.232861760990032,
0.631684198665438));
#13880=CARTESIAN_POINT('Ctrl Pts',(-0.722929908501543,-0.244251601209411,
0.663382628119203));
#13881=CARTESIAN_POINT('Ctrl Pts',(-0.707917883896095,-0.246942143572133,
0.679352081686668));
#13882=CARTESIAN_POINT('Ctrl Pts',(-0.679352081686668,-0.246942143572133,
0.707917883896095));
#13883=CARTESIAN_POINT('Ctrl Pts',(-0.663382628119203,-0.244251601209411,
0.722929908501544));
#13884=CARTESIAN_POINT('Ctrl Pts',(-0.631684198665438,-0.232861760990031,
0.750785745543687));
#13885=CARTESIAN_POINT('Ctrl Pts',(-0.615966552324775,-0.224161999508995,
0.763642258217233));
#13886=CARTESIAN_POINT('Ctrl Pts',(-0.587792702767295,-0.203463743702801,
0.78555112003688));
#13887=CARTESIAN_POINT('Ctrl Pts',(-0.573915184558107,-0.190326085855194,
0.795684265985088));
#13888=CARTESIAN_POINT('Ctrl Pts',(-0.548874290046456,-0.159766064500479,
0.813159949759));
#13889=CARTESIAN_POINT('Ctrl Pts',(-0.537715343527944,-0.142345102874864,
0.820511285096538));
#13890=CARTESIAN_POINT('Ctrl Pts',(-0.517157748491652,-0.0999305678883309,
0.833661031856294));
#13891=CARTESIAN_POINT('Ctrl Pts',(-0.508899795931835,-0.0740444353928835,
0.838633903678357));
#13892=CARTESIAN_POINT('Ctrl Pts',(-0.504455939115716,-0.04763,0.841298510752801));
#13893=CARTESIAN_POINT('Origin',(-0.707106781186548,-0.04763,0.707106781186547));
#13894=CARTESIAN_POINT('Origin',(0.,-0.04763,0.));
#13895=CARTESIAN_POINT('',(-0.951592097314,-0.04763,0.238183666596899));
#13896=CARTESIAN_POINT('Origin',(0.,-0.04763,0.));
#13897=CARTESIAN_POINT('Origin',(-1.,-0.04763,-1.11022302462516E-16));
#13898=CARTESIAN_POINT('Origin',(-1.,0.,-1.11022302462516E-16));
#13899=CARTESIAN_POINT('',(-0.951592097314,-0.04763,-0.2381836665969));
#13900=CARTESIAN_POINT('',(-0.980948,-0.246942143572133,1.08514323328844E-18));
#13901=CARTESIAN_POINT('Ctrl Pts',(-0.951592097314,-0.04763,-0.238183666596899));
#13902=CARTESIAN_POINT('Ctrl Pts',(-0.952850216871763,-0.0740444353928835,
-0.233157223576062));
#13903=CARTESIAN_POINT('Ctrl Pts',(-0.955173119738174,-0.0999305678883309,
-0.223801617934946));
#13904=CARTESIAN_POINT('Ctrl Pts',(-0.960411259488514,-0.142345102874864,
-0.199966927975188));
#13905=CARTESIAN_POINT('Ctrl Pts',(-0.963103647174702,-0.159766064500479,
-0.1868781821531));
#13906=CARTESIAN_POINT('Ctrl Pts',(-0.968453058988463,-0.190326085855194,
-0.15681442133453));
#13907=CARTESIAN_POINT('Ctrl Pts',(-0.971100730005489,-0.203463743702801,
-0.139836317888043));
#13908=CARTESIAN_POINT('Ctrl Pts',(-0.975530745318961,-0.224161999508995,
-0.104422493053067));
#13909=CARTESIAN_POINT('Ctrl Pts',(-0.977553872336861,-0.232861760990032,
-0.0842175114474175));
#13910=CARTESIAN_POINT('Ctrl Pts',(-0.980270995488453,-0.244251601209411,
-0.0421062857595699));
#13911=CARTESIAN_POINT('Ctrl Pts',(-0.980948,-0.246942143572133,-0.0201990724523195));
#13912=CARTESIAN_POINT('Ctrl Pts',(-0.980948,-0.246942143572133,-1.17961196366423E-16));
#13913=CARTESIAN_POINT('Origin',(-1.,-0.04763,-1.11022302462516E-16));
#13914=CARTESIAN_POINT('Ctrl Pts',(-0.980948,-0.246942143572133,-1.17961196366423E-16));
#13915=CARTESIAN_POINT('Ctrl Pts',(-0.980948,-0.246942143572133,0.0201990724523192));
#13916=CARTESIAN_POINT('Ctrl Pts',(-0.980270995488453,-0.244251601209411,
0.0421062857595695));
#13917=CARTESIAN_POINT('Ctrl Pts',(-0.977553872336861,-0.232861760990032,
0.0842175114474169));
#13918=CARTESIAN_POINT('Ctrl Pts',(-0.975530745318961,-0.224161999508995,
0.104422493053066));
#13919=CARTESIAN_POINT('Ctrl Pts',(-0.971100730005489,-0.203463743702801,
0.139836317888042));
#13920=CARTESIAN_POINT('Ctrl Pts',(-0.968453058988463,-0.190326085855194,
0.15681442133453));
#13921=CARTESIAN_POINT('Ctrl Pts',(-0.963103647174702,-0.15976606450048,
0.1868781821531));
#13922=CARTESIAN_POINT('Ctrl Pts',(-0.960411259488514,-0.142345102874864,
0.199966927975188));
#13923=CARTESIAN_POINT('Ctrl Pts',(-0.955173119738174,-0.099930567888331,
0.223801617934945));
#13924=CARTESIAN_POINT('Ctrl Pts',(-0.952850216871763,-0.0740444353928835,
0.233157223576061));
#13925=CARTESIAN_POINT('Ctrl Pts',(-0.951592097314,-0.04763,0.238183666596899));
#13926=CARTESIAN_POINT('Origin',(0.,-0.04763,0.));
#13927=CARTESIAN_POINT('',(-0.841298510752802,-0.04763,-0.504455939115715));
#13928=CARTESIAN_POINT('Origin',(0.,-0.04763,0.));
#13929=CARTESIAN_POINT('Origin',(-0.707106781186547,-0.04763,-0.707106781186548));
#13930=CARTESIAN_POINT('Origin',(-0.707106781186547,0.,-0.707106781186548));
#13931=CARTESIAN_POINT('',(-0.504455939115715,-0.04763,-0.841298510752802));
#13932=CARTESIAN_POINT('Ctrl Pts',(-0.504455939115715,-0.04763,-0.841298510752802));
#13933=CARTESIAN_POINT('Ctrl Pts',(-0.508899795931835,-0.0740444353928835,
-0.838633903678357));
#13934=CARTESIAN_POINT('Ctrl Pts',(-0.517157748491652,-0.0999305678883309,
-0.833661031856294));
#13935=CARTESIAN_POINT('Ctrl Pts',(-0.537715343527944,-0.142345102874864,
-0.820511285096538));
#13936=CARTESIAN_POINT('Ctrl Pts',(-0.548874290046456,-0.159766064500479,
-0.813159949759));
#13937=CARTESIAN_POINT('Ctrl Pts',(-0.573915184558107,-0.190326085855194,
-0.795684265985089));
#13938=CARTESIAN_POINT('Ctrl Pts',(-0.587792702767295,-0.203463743702801,
-0.78555112003688));
#13939=CARTESIAN_POINT('Ctrl Pts',(-0.615966552324775,-0.224161999508995,
-0.763642258217233));
#13940=CARTESIAN_POINT('Ctrl Pts',(-0.631684198665438,-0.232861760990032,
-0.750785745543687));
#13941=CARTESIAN_POINT('Ctrl Pts',(-0.663382628119203,-0.244251601209411,
-0.722929908501543));
#13942=CARTESIAN_POINT('Ctrl Pts',(-0.679352081686668,-0.246942143572133,
-0.707917883896095));
#13943=CARTESIAN_POINT('Ctrl Pts',(-0.707917883896095,-0.246942143572133,
-0.679352081686668));
#13944=CARTESIAN_POINT('Ctrl Pts',(-0.722929908501543,-0.244251601209411,
-0.663382628119203));
#13945=CARTESIAN_POINT('Ctrl Pts',(-0.750785745543687,-0.232861760990032,
-0.631684198665439));
#13946=CARTESIAN_POINT('Ctrl Pts',(-0.763642258217232,-0.224161999508995,
-0.615966552324775));
#13947=CARTESIAN_POINT('Ctrl Pts',(-0.78555112003688,-0.203463743702801,
-0.587792702767295));
#13948=CARTESIAN_POINT('Ctrl Pts',(-0.795684265985088,-0.190326085855194,
-0.573915184558107));
#13949=CARTESIAN_POINT('Ctrl Pts',(-0.813159949759,-0.15976606450048,-0.548874290046456));
#13950=CARTESIAN_POINT('Ctrl Pts',(-0.820511285096538,-0.142345102874864,
-0.537715343527944));
#13951=CARTESIAN_POINT('Ctrl Pts',(-0.833661031856294,-0.0999305678883311,
-0.517157748491652));
#13952=CARTESIAN_POINT('Ctrl Pts',(-0.838633903678357,-0.0740444353928836,
-0.508899795931835));
#13953=CARTESIAN_POINT('Ctrl Pts',(-0.841298510752801,-0.04763,-0.504455939115715));
#13954=CARTESIAN_POINT('Origin',(-0.707106781186547,-0.04763,-0.707106781186548));
#13955=CARTESIAN_POINT('Origin',(0.,-0.04763,0.));
#13956=CARTESIAN_POINT('',(-0.238183666596899,-0.04763,-0.951592097314));
#13957=CARTESIAN_POINT('Origin',(0.,-0.04763,0.));
#13958=CARTESIAN_POINT('Origin',(5.55111512312578E-17,-0.04763,-1.));
#13959=CARTESIAN_POINT('Origin',(5.55111512312578E-17,0.,-1.));
#13960=CARTESIAN_POINT('',(0.238183666596899,-0.04763,-0.951592097314));
#13961=CARTESIAN_POINT('Ctrl Pts',(0.238183666596899,-0.04763,-0.951592097314));
#13962=CARTESIAN_POINT('Ctrl Pts',(0.233157223576062,-0.0740444353928835,
-0.952850216871763));
#13963=CARTESIAN_POINT('Ctrl Pts',(0.223801617934946,-0.099930567888331,
-0.955173119738174));
#13964=CARTESIAN_POINT('Ctrl Pts',(0.199966927975188,-0.142345102874864,
-0.960411259488514));
#13965=CARTESIAN_POINT('Ctrl Pts',(0.1868781821531,-0.15976606450048,-0.963103647174702));
#13966=CARTESIAN_POINT('Ctrl Pts',(0.15681442133453,-0.190326085855194,
-0.968453058988463));
#13967=CARTESIAN_POINT('Ctrl Pts',(0.139836317888042,-0.203463743702801,
-0.971100730005489));
#13968=CARTESIAN_POINT('Ctrl Pts',(0.104422493053067,-0.224161999508995,
-0.975530745318961));
#13969=CARTESIAN_POINT('Ctrl Pts',(0.0842175114474173,-0.232861760990032,
-0.977553872336861));
#13970=CARTESIAN_POINT('Ctrl Pts',(0.0421062857595698,-0.244251601209411,
-0.980270995488453));
#13971=CARTESIAN_POINT('Ctrl Pts',(0.0201990724523194,-0.246942143572133,
-0.980948));
#13972=CARTESIAN_POINT('Ctrl Pts',(-0.0201990724523193,-0.246942143572133,
-0.980948));
#13973=CARTESIAN_POINT('Ctrl Pts',(-0.0421062857595697,-0.244251601209411,
-0.980270995488453));
#13974=CARTESIAN_POINT('Ctrl Pts',(-0.0842175114474171,-0.232861760990032,
-0.977553872336861));
#13975=CARTESIAN_POINT('Ctrl Pts',(-0.104422493053067,-0.224161999508995,
-0.975530745318961));
#13976=CARTESIAN_POINT('Ctrl Pts',(-0.139836317888042,-0.203463743702801,
-0.971100730005489));
#13977=CARTESIAN_POINT('Ctrl Pts',(-0.15681442133453,-0.190326085855194,
-0.968453058988463));
#13978=CARTESIAN_POINT('Ctrl Pts',(-0.1868781821531,-0.15976606450048,-0.963103647174702));
#13979=CARTESIAN_POINT('Ctrl Pts',(-0.199966927975188,-0.142345102874864,
-0.960411259488514));
#13980=CARTESIAN_POINT('Ctrl Pts',(-0.223801617934945,-0.099930567888331,
-0.955173119738174));
#13981=CARTESIAN_POINT('Ctrl Pts',(-0.233157223576062,-0.0740444353928835,
-0.952850216871763));
#13982=CARTESIAN_POINT('Ctrl Pts',(-0.238183666596899,-0.0476299999999999,
-0.951592097314));
#13983=CARTESIAN_POINT('Origin',(5.55111512312578E-17,-0.04763,-1.));
#13984=CARTESIAN_POINT('Origin',(0.,-0.04763,0.));
#13985=CARTESIAN_POINT('',(0.504455939115715,-0.04763,-0.841298510752802));
#13986=CARTESIAN_POINT('Origin',(0.,-0.04763,0.));
#13987=CARTESIAN_POINT('Origin',(0.707106781186548,-0.04763,-0.707106781186547));
#13988=CARTESIAN_POINT('Origin',(0.707106781186548,0.,-0.707106781186547));
#13989=CARTESIAN_POINT('',(0.841298510752802,-0.04763,-0.504455939115715));
#13990=CARTESIAN_POINT('Ctrl Pts',(0.841298510752802,-0.04763,-0.504455939115715));
#13991=CARTESIAN_POINT('Ctrl Pts',(0.838633903678357,-0.0740444353928835,
-0.508899795931835));
#13992=CARTESIAN_POINT('Ctrl Pts',(0.833661031856294,-0.0999305678883309,
-0.517157748491652));
#13993=CARTESIAN_POINT('Ctrl Pts',(0.820511285096538,-0.142345102874864,
-0.537715343527944));
#13994=CARTESIAN_POINT('Ctrl Pts',(0.813159949759,-0.159766064500479,-0.548874290046456));
#13995=CARTESIAN_POINT('Ctrl Pts',(0.795684265985088,-0.190326085855194,
-0.573915184558107));
#13996=CARTESIAN_POINT('Ctrl Pts',(0.78555112003688,-0.203463743702801,
-0.587792702767295));
#13997=CARTESIAN_POINT('Ctrl Pts',(0.763642258217233,-0.224161999508995,
-0.615966552324775));
#13998=CARTESIAN_POINT('Ctrl Pts',(0.750785745543687,-0.232861760990032,
-0.631684198665438));
#13999=CARTESIAN_POINT('Ctrl Pts',(0.722929908501543,-0.244251601209411,
-0.663382628119203));
#14000=CARTESIAN_POINT('Ctrl Pts',(0.707917883896095,-0.246942143572133,
-0.679352081686668));
#14001=CARTESIAN_POINT('Ctrl Pts',(0.679352081686668,-0.246942143572133,
-0.707917883896095));
#14002=CARTESIAN_POINT('Ctrl Pts',(0.663382628119203,-0.244251601209411,
-0.722929908501543));
#14003=CARTESIAN_POINT('Ctrl Pts',(0.631684198665438,-0.232861760990032,
-0.750785745543687));
#14004=CARTESIAN_POINT('Ctrl Pts',(0.615966552324775,-0.224161999508995,
-0.763642258217232));
#14005=CARTESIAN_POINT('Ctrl Pts',(0.587792702767295,-0.203463743702801,
-0.78555112003688));
#14006=CARTESIAN_POINT('Ctrl Pts',(0.573915184558107,-0.190326085855194,
-0.795684265985088));
#14007=CARTESIAN_POINT('Ctrl Pts',(0.548874290046456,-0.159766064500479,
-0.813159949759));
#14008=CARTESIAN_POINT('Ctrl Pts',(0.537715343527944,-0.142345102874864,
-0.820511285096538));
#14009=CARTESIAN_POINT('Ctrl Pts',(0.517157748491652,-0.099930567888331,
-0.833661031856294));
#14010=CARTESIAN_POINT('Ctrl Pts',(0.508899795931835,-0.0740444353928835,
-0.838633903678357));
#14011=CARTESIAN_POINT('Ctrl Pts',(0.504455939115715,-0.04763,-0.841298510752801));
#14012=CARTESIAN_POINT('Origin',(0.707106781186548,-0.04763,-0.707106781186547));
#14013=CARTESIAN_POINT('Origin',(0.,-0.166705,0.));
#14014=CARTESIAN_POINT('',(-0.980948,-0.28578,1.20131482833E-16));
#14015=CARTESIAN_POINT('Origin',(0.,-0.28578,0.));
#14016=CARTESIAN_POINT('',(-0.980948,-0.166705,1.20131482833E-16));
#14017=CARTESIAN_POINT('',(0.951592097314,-0.04763,0.238183666596899));
#14018=CARTESIAN_POINT('Origin',(0.,-0.04763,0.));
#14019=CARTESIAN_POINT('',(0.951592097314,-0.04763,-0.238183666596899));
#14020=CARTESIAN_POINT('Ctrl Pts',(0.951592097314,-0.04763,0.238183666596899));
#14021=CARTESIAN_POINT('Ctrl Pts',(0.952850216871763,-0.0740444353928835,
0.233157223576062));
#14022=CARTESIAN_POINT('Ctrl Pts',(0.955173119738174,-0.099930567888331,
0.223801617934945));
#14023=CARTESIAN_POINT('Ctrl Pts',(0.960411259488514,-0.142345102874864,
0.199966927975188));
#14024=CARTESIAN_POINT('Ctrl Pts',(0.963103647174702,-0.15976606450048,
0.1868781821531));
#14025=CARTESIAN_POINT('Ctrl Pts',(0.968453058988463,-0.190326085855194,
0.15681442133453));
#14026=CARTESIAN_POINT('Ctrl Pts',(0.971100730005489,-0.203463743702801,
0.139836317888042));
#14027=CARTESIAN_POINT('Ctrl Pts',(0.975530745318961,-0.224161999508995,
0.104422493053067));
#14028=CARTESIAN_POINT('Ctrl Pts',(0.977553872336861,-0.232861760990032,
0.0842175114474172));
#14029=CARTESIAN_POINT('Ctrl Pts',(0.980270995488453,-0.244251601209411,
0.0421062857595697));
#14030=CARTESIAN_POINT('Ctrl Pts',(0.980948,-0.246942143572133,0.0201990724523194));
#14031=CARTESIAN_POINT('Ctrl Pts',(0.980948,-0.246942143572133,-0.0201990724523194));
#14032=CARTESIAN_POINT('Ctrl Pts',(0.980270995488453,-0.244251601209411,
-0.0421062857595697));
#14033=CARTESIAN_POINT('Ctrl Pts',(0.977553872336861,-0.232861760990032,
-0.0842175114474172));
#14034=CARTESIAN_POINT('Ctrl Pts',(0.975530745318961,-0.224161999508995,
-0.104422493053067));
#14035=CARTESIAN_POINT('Ctrl Pts',(0.971100730005489,-0.203463743702801,
-0.139836317888042));
#14036=CARTESIAN_POINT('Ctrl Pts',(0.968453058988463,-0.190326085855194,
-0.15681442133453));
#14037=CARTESIAN_POINT('Ctrl Pts',(0.963103647174702,-0.15976606450048,
-0.1868781821531));
#14038=CARTESIAN_POINT('Ctrl Pts',(0.960411259488514,-0.142345102874864,
-0.199966927975188));
#14039=CARTESIAN_POINT('Ctrl Pts',(0.955173119738174,-0.099930567888331,
-0.223801617934945));
#14040=CARTESIAN_POINT('Ctrl Pts',(0.952850216871763,-0.0740444353928835,
-0.233157223576062));
#14041=CARTESIAN_POINT('Ctrl Pts',(0.951592097314,-0.0476299999999999,-0.238183666596899));
#14042=CARTESIAN_POINT('Origin',(0.,-0.04763,0.));
#14043=CARTESIAN_POINT('Origin',(0.,-0.04763,0.));
#14044=CARTESIAN_POINT('Origin',(1.,-0.04763,0.));
#14045=CARTESIAN_POINT('Origin',(1.,0.,0.));
#14046=CARTESIAN_POINT('Origin',(1.,-0.04763,0.));
#14047=CARTESIAN_POINT('Origin',(0.,-0.28578,0.));
#14048=CARTESIAN_POINT('Origin',(0.,-0.04763,0.));
#14049=CARTESIAN_POINT('',(0.,0.,0.));
#14050=CARTESIAN_POINT('Origin',(1.013815,0.445,0.));
#14051=CARTESIAN_POINT('',(-1.013815,0.445,-1.24156529467757E-16));
#14052=CARTESIAN_POINT('Origin',(0.,0.445,0.));
#14053=CARTESIAN_POINT('',(-0.991185,0.445,-1.21385153761287E-16));
#14054=CARTESIAN_POINT('Origin',(0.,0.445,0.));
#14055=CARTESIAN_POINT('Origin',(0.,0.4075,0.));
#14056=CARTESIAN_POINT('',(-1.013815,0.37,-1.24156529467757E-16));
#14057=CARTESIAN_POINT('Origin',(0.,0.37,0.));
#14058=CARTESIAN_POINT('',(-1.013815,0.4075,-1.24156529467757E-16));
#14059=CARTESIAN_POINT('Origin',(0.991185,0.37,0.));
#14060=CARTESIAN_POINT('',(-0.991185,0.37,-1.21385153761287E-16));
#14061=CARTESIAN_POINT('Origin',(0.,0.37,0.));
#14062=CARTESIAN_POINT('Origin',(0.,0.4075,0.));
#14063=CARTESIAN_POINT('',(-0.991185,0.4075,-1.21385153761287E-16));
#14064=CARTESIAN_POINT('Origin',(1.013815,-0.37,0.));
#14065=CARTESIAN_POINT('',(-1.013815,-0.37,-1.24156529467757E-16));
#14066=CARTESIAN_POINT('Origin',(0.,-0.37,0.));
#14067=CARTESIAN_POINT('',(-0.991185,-0.37,-1.21385153761287E-16));
#14068=CARTESIAN_POINT('Origin',(0.,-0.37,0.));
#14069=CARTESIAN_POINT('Origin',(0.,-0.4075,0.));
#14070=CARTESIAN_POINT('',(-1.013815,-0.445,-1.24156529467757E-16));
#14071=CARTESIAN_POINT('Origin',(0.,-0.445,0.));
#14072=CARTESIAN_POINT('',(-1.013815,-0.4075,-1.24156529467757E-16));
#14073=CARTESIAN_POINT('Origin',(0.991185,-0.445,0.));
#14074=CARTESIAN_POINT('',(-0.991185,-0.445,-1.21385153761287E-16));
#14075=CARTESIAN_POINT('Origin',(0.,-0.445,0.));
#14076=CARTESIAN_POINT('Origin',(0.,-0.4075,0.));
#14077=CARTESIAN_POINT('',(-0.991185,-0.4075,-1.21385153761287E-16));
#14078=CARTESIAN_POINT('',(0.,0.,0.));
#14079=CARTESIAN_POINT('',(0.,0.,0.));
#14080=CARTESIAN_POINT('',(0.,0.,0.));
#14081=CARTESIAN_POINT('',(0.,0.,0.));
#14082=CARTESIAN_POINT('',(0.,0.,0.));
#14083=CARTESIAN_POINT('',(0.,0.,0.));
#14084=CARTESIAN_POINT('',(0.,0.,0.));
#14085=CARTESIAN_POINT('Origin',(0.75,1.2,0.));
#14086=CARTESIAN_POINT('',(0.885663593019381,1.2,-0.16));
#14087=CARTESIAN_POINT('',(0.885663593019381,1.2,0.16));
#14088=CARTESIAN_POINT('Origin',(0.,1.2,0.));
#14089=CARTESIAN_POINT('',(0.93,1.2,-0.16));
#14090=CARTESIAN_POINT('',(0.93,1.2,-0.16));
#14091=CARTESIAN_POINT('',(0.93,1.2,0.16));
#14092=CARTESIAN_POINT('',(0.93,1.2,0.16));
#14093=CARTESIAN_POINT('',(0.57,1.2,0.16));
#14094=CARTESIAN_POINT('Origin',(0.57,0.,0.16));
#14095=CARTESIAN_POINT('',(0.885663593019381,-1.2,0.16));
#14096=CARTESIAN_POINT('',(0.885663593019381,0.,0.16));
#14097=CARTESIAN_POINT('',(0.93,-1.2,0.16));
#14098=CARTESIAN_POINT('',(0.93,0.,0.16));
#14099=CARTESIAN_POINT('',(0.57,-1.2,0.16));
#14100=CARTESIAN_POINT('Origin',(0.75,-1.2,0.));
#14101=CARTESIAN_POINT('',(0.885663593019381,-1.2,-0.16));
#14102=CARTESIAN_POINT('Origin',(0.,-1.2,0.));
#14103=CARTESIAN_POINT('',(0.93,-1.2,-0.16));
#14104=CARTESIAN_POINT('',(0.93,-1.2,0.16));
#14105=CARTESIAN_POINT('',(0.93,-1.2,-0.16));
#14106=CARTESIAN_POINT('Origin',(0.93,0.,-0.16));
#14107=CARTESIAN_POINT('',(0.885663593019381,0.,-0.16));
#14108=CARTESIAN_POINT('',(0.93,0.,-0.16));
#14109=CARTESIAN_POINT('Origin',(0.93,0.,0.16));
#14110=CARTESIAN_POINT('Origin',(1.05,1.5,0.));
#14111=CARTESIAN_POINT('',(-1.05,1.5,-1.28587913910472E-16));
#14112=CARTESIAN_POINT('Origin',(0.,1.5,0.));
#14113=CARTESIAN_POINT('',(-0.9,1.5,-1.10218211923262E-16));
#14114=CARTESIAN_POINT('Origin',(0.,1.5,0.));
#14115=CARTESIAN_POINT('Origin',(0.,1.315,0.));
#14116=CARTESIAN_POINT('',(-1.05,1.13,-1.28587913910472E-16));
#14117=CARTESIAN_POINT('Origin',(0.,1.13,0.));
#14118=CARTESIAN_POINT('',(-1.05,1.315,-1.28587913910472E-16));
#14119=CARTESIAN_POINT('Origin',(1.,1.13,0.));
#14120=CARTESIAN_POINT('',(-1.,1.13,-1.22464679914735E-16));
#14121=CARTESIAN_POINT('Origin',(0.,1.13,0.));
#14122=CARTESIAN_POINT('Origin',(0.,1.065,0.));
#14123=CARTESIAN_POINT('',(-1.,1.,-1.22464679914735E-16));
#14124=CARTESIAN_POINT('Origin',(0.,1.,0.));
#14125=CARTESIAN_POINT('',(-1.,1.065,-1.22464679914735E-16));
#14126=CARTESIAN_POINT('Origin',(1.05,1.,0.));
#14127=CARTESIAN_POINT('',(-1.05,1.,-1.28587913910472E-16));
#14128=CARTESIAN_POINT('Origin',(0.,1.,0.));
#14129=CARTESIAN_POINT('Origin',(0.,0.,0.));
#14130=CARTESIAN_POINT('',(-1.05,-1.,-1.28587913910472E-16));
#14131=CARTESIAN_POINT('Origin',(0.,-1.,0.));
#14132=CARTESIAN_POINT('',(-1.05,0.,-1.28587913910472E-16));
#14133=CARTESIAN_POINT('Origin',(1.,-1.,0.));
#14134=CARTESIAN_POINT('',(-1.,-1.,-1.22464679914735E-16));
#14135=CARTESIAN_POINT('Origin',(0.,-1.,0.));
#14136=CARTESIAN_POINT('Origin',(0.,-1.065,0.));
#14137=CARTESIAN_POINT('',(-1.,-1.13,-1.22464679914735E-16));
#14138=CARTESIAN_POINT('Origin',(0.,-1.13,0.));
#14139=CARTESIAN_POINT('',(-1.,-1.065,-1.22464679914735E-16));
#14140=CARTESIAN_POINT('Origin',(1.05,-1.13,0.));
#14141=CARTESIAN_POINT('',(-1.05,-1.13,-1.28587913910472E-16));
#14142=CARTESIAN_POINT('Origin',(0.,-1.13,0.));
#14143=CARTESIAN_POINT('Origin',(0.,-1.315,0.));
#14144=CARTESIAN_POINT('',(-1.05,-1.5,-1.28587913910472E-16));
#14145=CARTESIAN_POINT('Origin',(0.,-1.5,0.));
#14146=CARTESIAN_POINT('',(-1.05,-1.315,-1.28587913910472E-16));
#14147=CARTESIAN_POINT('Origin',(0.9,-1.5,0.));
#14148=CARTESIAN_POINT('',(-0.9,-1.5,-1.10218211923262E-16));
#14149=CARTESIAN_POINT('Origin',(0.,-1.5,0.));
#14150=CARTESIAN_POINT('Origin',(0.,0.,0.));
#14151=CARTESIAN_POINT('',(-0.9,0.,-1.10218211923262E-16));
#14152=CARTESIAN_POINT('',(0.,0.,0.));
#14153=CARTESIAN_POINT('Origin',(0.75,1.2,0.));
#14154=CARTESIAN_POINT('',(0.880582193778639,1.2,0.16));
#14155=CARTESIAN_POINT('',(0.880582193778639,1.2,-0.16));
#14156=CARTESIAN_POINT('Origin',(0.,1.2,0.));
#14157=CARTESIAN_POINT('',(0.583459510163302,1.2,0.16));
#14158=CARTESIAN_POINT('',(0.57,1.2,0.16));
#14159=CARTESIAN_POINT('',(0.583459510163302,1.2,-0.16));
#14160=CARTESIAN_POINT('Origin',(0.,1.2,0.));
#14161=CARTESIAN_POINT('',(0.93,1.2,-0.16));
#14162=CARTESIAN_POINT('Origin',(0.93,0.,-0.16));
#14163=CARTESIAN_POINT('',(0.880582193778639,-1.2,-0.16));
#14164=CARTESIAN_POINT('',(0.880582193778639,0.,-0.16));
#14165=CARTESIAN_POINT('',(0.583459510163302,-1.2,-0.16));
#14166=CARTESIAN_POINT('',(0.583459510163302,0.,-0.16));
#14167=CARTESIAN_POINT('',(0.93,-1.2,-0.16));
#14168=CARTESIAN_POINT('Origin',(0.75,-1.2,0.));
#14169=CARTESIAN_POINT('',(0.880582193778639,-1.2,0.16));
#14170=CARTESIAN_POINT('Origin',(0.,-1.2,0.));
#14171=CARTESIAN_POINT('',(0.583459510163302,-1.2,0.16));
#14172=CARTESIAN_POINT('Origin',(0.,-1.2,0.));
#14173=CARTESIAN_POINT('',(0.57,-1.2,0.16));
#14174=CARTESIAN_POINT('Origin',(0.57,0.,0.16));
#14175=CARTESIAN_POINT('',(0.880582193778639,0.,0.16));
#14176=CARTESIAN_POINT('',(0.583459510163302,0.,0.16));
#14177=CARTESIAN_POINT('Origin',(0.895,1.35,0.));
#14178=CARTESIAN_POINT('',(-0.895,1.35,-1.09605888523688E-16));
#14179=CARTESIAN_POINT('Origin',(0.,1.35,0.));
#14180=CARTESIAN_POINT('',(-0.605,1.35,-7.40911313484149E-17));
#14181=CARTESIAN_POINT('Origin',(0.,1.35,0.));
#14182=CARTESIAN_POINT('Origin',(0.,0.,0.));
#14183=CARTESIAN_POINT('',(-0.895,-1.35,-1.09605888523688E-16));
#14184=CARTESIAN_POINT('Origin',(0.,-1.35,0.));
#14185=CARTESIAN_POINT('',(-0.895,0.,-1.09605888523688E-16));
#14186=CARTESIAN_POINT('Origin',(0.605,-1.35,0.));
#14187=CARTESIAN_POINT('',(-0.605,-1.35,-7.40911313484149E-17));
#14188=CARTESIAN_POINT('Origin',(0.,-1.35,0.));
#14189=CARTESIAN_POINT('Origin',(0.,0.,0.));
#14190=CARTESIAN_POINT('',(-0.605,0.,-7.40911313484149E-17));
#14191=CARTESIAN_POINT('',(0.,0.,0.));
#14192=CARTESIAN_POINT('',(0.,0.,0.));
#14193=CARTESIAN_POINT('',(0.,0.,0.));
#14194=CARTESIAN_POINT('Origin',(0.0866025403784439,-0.4,-0.15));
#14195=CARTESIAN_POINT('',(0.173205080756888,-0.4,0.));
#14196=CARTESIAN_POINT('',(0.0866025403784439,-0.4,-0.15));
#14197=CARTESIAN_POINT('',(0.173205080756888,-0.4,0.));
#14198=CARTESIAN_POINT('',(0.0866025403784439,-0.64,-0.15));
#14199=CARTESIAN_POINT('',(0.0866025403784439,-0.4,-0.15));
#14200=CARTESIAN_POINT('',(0.173205080756888,-0.64,0.));
#14201=CARTESIAN_POINT('',(0.173205080756888,-0.64,0.));
#14202=CARTESIAN_POINT('',(0.173205080756888,-0.4,0.));
#14203=CARTESIAN_POINT('Origin',(-0.0866025403784438,-0.4,-0.15));
#14204=CARTESIAN_POINT('',(-0.0866025403784438,-0.4,-0.15));
#14205=CARTESIAN_POINT('',(0.0866025403784439,-0.4,-0.15));
#14206=CARTESIAN_POINT('',(-0.0866025403784438,-0.64,-0.15));
#14207=CARTESIAN_POINT('',(-0.0866025403784438,-0.4,-0.15));
#14208=CARTESIAN_POINT('',(0.0866025403784439,-0.64,-0.15));
#14209=CARTESIAN_POINT('Origin',(-0.173205080756888,-0.4,-2.77555756156289E-17));
#14210=CARTESIAN_POINT('',(-0.173205080756888,-0.4,-2.12115047744981E-17));
#14211=CARTESIAN_POINT('',(-0.0866025403784438,-0.4,-0.15));
#14212=CARTESIAN_POINT('',(-0.173205080756888,-0.64,-2.77555756156289E-17));
#14213=CARTESIAN_POINT('',(-0.173205080756888,-0.4,-2.12115047744981E-17));
#14214=CARTESIAN_POINT('',(-0.0866025403784438,-0.64,-0.15));
#14215=CARTESIAN_POINT('Origin',(-0.0866025403784439,-0.4,0.15));
#14216=CARTESIAN_POINT('',(-0.0866025403784439,-0.4,0.15));
#14217=CARTESIAN_POINT('',(-0.173205080756888,-0.4,-2.12115047744981E-17));
#14218=CARTESIAN_POINT('',(-0.0866025403784439,-0.64,0.15));
#14219=CARTESIAN_POINT('',(-0.0866025403784439,-0.4,0.15));
#14220=CARTESIAN_POINT('',(-0.173205080756888,-0.64,-2.12115047744981E-17));
#14221=CARTESIAN_POINT('Origin',(0.0866025403784439,-0.4,0.15));
#14222=CARTESIAN_POINT('',(0.0866025403784439,-0.4,0.15));
#14223=CARTESIAN_POINT('',(-0.0866025403784439,-0.4,0.15));
#14224=CARTESIAN_POINT('',(0.0866025403784439,-0.64,0.15));
#14225=CARTESIAN_POINT('',(0.0866025403784439,-0.4,0.15));
#14226=CARTESIAN_POINT('',(-0.0866025403784439,-0.64,0.15));
#14227=CARTESIAN_POINT('Origin',(0.173205080756888,-0.4,0.));
#14228=CARTESIAN_POINT('',(0.0866025403784439,-0.4,0.15));
#14229=CARTESIAN_POINT('',(0.0866025403784439,-0.64,0.15));
#14230=CARTESIAN_POINT('Origin',(0.,-0.4,-2.77555756156289E-17));
#14231=CARTESIAN_POINT('Origin',(0.,-0.64,-2.77555756156289E-17));
#14232=CARTESIAN_POINT('Origin',(0.,-1.6,0.));
#14233=CARTESIAN_POINT('',(-0.2,-1.6,2.44929359829471E-17));
#14234=CARTESIAN_POINT('Origin',(0.,-1.6,0.));
#14235=CARTESIAN_POINT('',(-0.16,-1.6,-1.95943487863577E-17));
#14236=CARTESIAN_POINT('Origin',(0.,-1.6,0.));
#14237=CARTESIAN_POINT('Origin',(0.,-3.,0.));
#14238=CARTESIAN_POINT('',(-0.2,-3.,2.44929359829471E-17));
#14239=CARTESIAN_POINT('',(-0.2,-3.,2.44929359829471E-17));
#14240=CARTESIAN_POINT('Origin',(0.,-3.,0.));
#14241=CARTESIAN_POINT('Origin',(0.,-3.,0.));
#14242=CARTESIAN_POINT('Origin',(0.3,0.4,0.));
#14243=CARTESIAN_POINT('',(-0.3,0.4,-3.67394039744206E-17));
#14244=CARTESIAN_POINT('Origin',(0.,0.4,0.));
#14245=CARTESIAN_POINT('Origin',(0.,0.375,0.));
#14246=CARTESIAN_POINT('',(-0.35,0.35,-4.28626379701573E-17));
#14247=CARTESIAN_POINT('Origin',(0.,0.35,0.));
#14248=CARTESIAN_POINT('',(-0.325,0.375,-3.9801020972289E-17));
#14249=CARTESIAN_POINT('Origin',(0.,0.19,0.));
#14250=CARTESIAN_POINT('',(-0.35,0.03,-4.28626379701574E-17));
#14251=CARTESIAN_POINT('Origin',(0.,0.03,0.));
#14252=CARTESIAN_POINT('',(-0.35,0.19,-4.28626379701574E-17));
#14253=CARTESIAN_POINT('Origin',(0.,0.0149999999999999,0.));
#14254=CARTESIAN_POINT('',(-0.32,-3.29597460435593E-17,-3.91886975727153E-17));
#14255=CARTESIAN_POINT('Origin',(0.,0.,0.));
#14256=CARTESIAN_POINT('',(-0.335,0.0149999999999999,-4.10256677714363E-17));
#14257=CARTESIAN_POINT('Origin',(0.22,0.,0.));
#14258=CARTESIAN_POINT('',(-0.22,-6.93889390390723E-18,-2.69422295812418E-17));
#14259=CARTESIAN_POINT('Origin',(0.,0.,0.));
#14260=CARTESIAN_POINT('Origin',(0.,-0.02,0.));
#14261=CARTESIAN_POINT('',(-0.1954,-0.0492,2.39295984553393E-17));
#14262=CARTESIAN_POINT('Origin',(0.,-0.0492,0.));
#14263=CARTESIAN_POINT('',(-0.21,-0.02,-2.57175827820944E-17));
#14264=CARTESIAN_POINT('Origin',(0.,-0.8,0.));
#14265=CARTESIAN_POINT('',(-0.1954,-1.5646,2.39295984553393E-17));
#14266=CARTESIAN_POINT('Origin',(0.,-1.5646,0.));
#14267=CARTESIAN_POINT('',(-0.1954,-0.8,-2.39295984553393E-17));
#14268=CARTESIAN_POINT('Origin',(0.,-1.58,0.));
#14269=CARTESIAN_POINT('',(-0.18,-1.58,-2.20436423846524E-17));
#14270=CARTESIAN_POINT('',(0.,0.,0.));
#14271=CARTESIAN_POINT('',(0.,0.,0.));
#14272=CARTESIAN_POINT('Origin',(-2.82632109303527,-3.6,8.79263101785268));
#14273=CARTESIAN_POINT('',(-3.13132109303527,-3.5,8.79263101785268));
#14274=CARTESIAN_POINT('Origin',(-2.82632109303527,-3.5,8.79263101785268));
#14275=CARTESIAN_POINT('',(-3.13132109303527,-2.7,8.79263101785268));
#14276=CARTESIAN_POINT('',(-3.13132109303527,-3.6,8.79263101785268));
#14277=CARTESIAN_POINT('Origin',(-2.82632109303527,-2.7,8.79263101785268));
#14278=CARTESIAN_POINT('Origin',(-6.81682937671534,-3.5,16.2976855571536));
#14279=CARTESIAN_POINT('',(-6.1383908997902,-2.7,15.873750145767));
#14280=CARTESIAN_POINT('',(-6.1383908997902,-3.5,15.873750145767));
#14281=CARTESIAN_POINT('',(-6.1383908997902,-3.5,15.873750145767));
#14282=CARTESIAN_POINT('',(-6.84474897407734,-2.7,15.4981728955383));
#14283=CARTESIAN_POINT('Origin',(-6.81682937671534,-2.7,16.2976855571536));
#14284=CARTESIAN_POINT('',(-6.84474897407734,-3.5,15.4981728955383));
#14285=CARTESIAN_POINT('',(-6.84474897407734,-3.5,15.4981728955383));
#14286=CARTESIAN_POINT('Origin',(-6.81682937671534,-3.5,16.2976855571536));
#14287=CARTESIAN_POINT('Origin',(-4.,-3.5,11.));
#14288=CARTESIAN_POINT('',(-4.78345683176268,-3.5,11.6214462106767));
#14289=CARTESIAN_POINT('',(-4.35317903714357,-3.5,10.8122113748856));
#14290=CARTESIAN_POINT('',(-5.,-3.5,11.));
#14291=CARTESIAN_POINT('Origin',(-4.,-3.5,11.));
#14292=CARTESIAN_POINT('',(-3.92290124252446,-3.5,10.0029765390946));
#14293=CARTESIAN_POINT('Origin',(-4.,-3.5,11.));
#14294=CARTESIAN_POINT('',(-3.44919101049801,-3.5,9.11205716881713));
#14295=CARTESIAN_POINT('',(-3.17950013017884,-3.5,8.60484239273833));
#14296=CARTESIAN_POINT('',(-2.74283293621087,-3.5,9.48763441904585));
#14297=CARTESIAN_POINT('Origin',(-2.82632109303527,-3.5,8.79263101785268));
#14298=CARTESIAN_POINT('',(-3.21654316823732,-3.5,10.3785537893233));
#14299=CARTESIAN_POINT('',(-3.64682096285643,-3.5,11.1877886251144));
#14300=CARTESIAN_POINT('',(-4.07709875747554,-3.5,11.9970234609054));
#14301=CARTESIAN_POINT('Origin',(-4.,-3.5,11.));
#14302=CARTESIAN_POINT('',(-6.46365033957177,-3.5,16.4854741822679));
#14303=CARTESIAN_POINT('',(-4.5,-3.5,11.));
#14304=CARTESIAN_POINT('Origin',(-4.,-3.5,11.));
#14305=CARTESIAN_POINT('Origin',(-4.35317903714357,-3.5,10.8122113748856));
#14306=CARTESIAN_POINT('',(-4.78345683176268,-2.7,11.6214462106767));
#14307=CARTESIAN_POINT('',(-4.35317903714357,-2.7,10.8122113748856));
#14308=CARTESIAN_POINT('',(-4.78345683176268,-3.5,11.6214462106767));
#14309=CARTESIAN_POINT('Origin',(-5.40841468835767,-2.7,13.6488427785768));
#14310=CARTESIAN_POINT('',(-4.07709875747554,-2.7,11.9970234609054));
#14311=CARTESIAN_POINT('',(-6.46365033957177,-2.7,16.4854741822679));
#14312=CARTESIAN_POINT('Origin',(-4.,-2.7,11.));
#14313=CARTESIAN_POINT('Origin',(-6.46365033957177,-3.5,16.4854741822679));
#14314=CARTESIAN_POINT('',(-4.07709875747554,-3.5,11.9970234609054));
#14315=CARTESIAN_POINT('Origin',(-2.82632109303527,-3.5,8.79263101785268));
#14316=CARTESIAN_POINT('',(-3.44919101049801,-2.7,9.11205716881713));
#14317=CARTESIAN_POINT('',(-3.44919101049801,-3.5,9.11205716881713));
#14318=CARTESIAN_POINT('',(-2.74283293621087,-2.7,9.48763441904585));
#14319=CARTESIAN_POINT('Origin',(-2.82632109303527,-2.7,8.79263101785268));
#14320=CARTESIAN_POINT('',(-2.74283293621087,-3.5,9.48763441904585));
#14321=CARTESIAN_POINT('Origin',(-3.64682096285643,-3.5,11.1877886251144));
#14322=CARTESIAN_POINT('',(-3.21654316823732,-2.7,10.3785537893233));
#14323=CARTESIAN_POINT('',(-3.64682096285643,-2.7,11.1877886251144));
#14324=CARTESIAN_POINT('',(-3.21654316823732,-3.5,10.3785537893233));
#14325=CARTESIAN_POINT('Origin',(-3.41316054651764,-2.7,9.89631550892634));
#14326=CARTESIAN_POINT('',(-3.92290124252446,-2.7,10.0029765390946));
#14327=CARTESIAN_POINT('',(-3.17950013017884,-2.7,8.60484239273833));
#14328=CARTESIAN_POINT('Origin',(-4.,-2.7,11.));
#14329=CARTESIAN_POINT('Origin',(-3.17950013017884,-3.5,8.60484239273833));
#14330=CARTESIAN_POINT('',(-3.92290124252446,-3.5,10.0029765390946));
#14331=CARTESIAN_POINT('Origin',(-4.,-2.,11.));
#14332=CARTESIAN_POINT('',(-5.,-2.,11.));
#14333=CARTESIAN_POINT('Origin',(-4.,-2.,11.));
#14334=CARTESIAN_POINT('',(-4.7,-2.,11.));
#14335=CARTESIAN_POINT('Origin',(-4.,-2.,11.));
#14336=CARTESIAN_POINT('Origin',(-4.,-3.5,11.));
#14337=CARTESIAN_POINT('',(-5.,-3.5,11.));
#14338=CARTESIAN_POINT('Origin',(-4.,-0.45,11.));
#14339=CARTESIAN_POINT('',(-4.7,-0.45,11.));
#14340=CARTESIAN_POINT('Origin',(-4.,-0.45,11.));
#14341=CARTESIAN_POINT('',(-4.5,-0.45,11.));
#14342=CARTESIAN_POINT('Origin',(-4.,-0.45,11.));
#14343=CARTESIAN_POINT('Origin',(-4.,-2.,11.));
#14344=CARTESIAN_POINT('',(-4.7,-2.,11.));
#14345=CARTESIAN_POINT('Origin',(-4.,-4.,11.));
#14346=CARTESIAN_POINT('',(-4.5,-4.,11.));
#14347=CARTESIAN_POINT('',(-4.5,-4.,11.));
#14348=CARTESIAN_POINT('Origin',(-4.,-4.,11.));
#14349=CARTESIAN_POINT('Origin',(-4.,-4.,11.));
#14350=CARTESIAN_POINT('',(-4.5,1.8,11.));
#14351=CARTESIAN_POINT('Origin',(-4.,1.8,11.));
#14352=CARTESIAN_POINT('',(-4.5,-4.,11.));
#14353=CARTESIAN_POINT('Origin',(-4.,1.8,11.));
#14354=CARTESIAN_POINT('Origin',(-4.,-4.,11.));
#14355=CARTESIAN_POINT('',(0.,0.,0.));
#14356=CARTESIAN_POINT('Origin',(-4.,0.45,11.));
#14357=CARTESIAN_POINT('',(-4.505,1.,11.));
#14358=CARTESIAN_POINT('Origin',(-4.,1.,11.));
#14359=CARTESIAN_POINT('',(-4.505,0.45,11.));
#14360=CARTESIAN_POINT('',(-4.505,0.45,11.));
#14361=CARTESIAN_POINT('Origin',(-4.,0.45,11.));
#14362=CARTESIAN_POINT('Origin',(-4.,0.45,11.));
#14363=CARTESIAN_POINT('',(-4.7,1.,11.));
#14364=CARTESIAN_POINT('Origin',(-4.,1.,11.));
#14365=CARTESIAN_POINT('',(-4.7,0.45,11.));
#14366=CARTESIAN_POINT('',(-4.7,0.45,11.));
#14367=CARTESIAN_POINT('Origin',(-4.,0.45,11.));
#14368=CARTESIAN_POINT('Origin',(-4.,1.,11.));
#14369=CARTESIAN_POINT('Origin',(-4.,0.45,11.));
#14370=CARTESIAN_POINT('',(0.,0.,0.));
#14371=CARTESIAN_POINT('Origin',(-3.51,1.4,11.));
#14372=CARTESIAN_POINT('',(-3.51,1.28909463493591,10.8778320827713));
#14373=CARTESIAN_POINT('',(-3.51,1.51090536506409,10.8778320827713));
#14374=CARTESIAN_POINT('',(-3.51,1.,10.8778320827713));
#14375=CARTESIAN_POINT('Origin',(-3.51,1.4,11.));
#14376=CARTESIAN_POINT('Origin',(-3.51,1.4,11.));
#14377=CARTESIAN_POINT('',(-3.51,1.28909463493591,11.1221679172287));
#14378=CARTESIAN_POINT('Ctrl Pts',(-3.51,1.28909463493591,11.1221679172287));
#14379=CARTESIAN_POINT('Ctrl Pts',(-3.50955146832001,1.28711294069536,11.1203689136263));
#14380=CARTESIAN_POINT('Ctrl Pts',(-3.50910475462832,1.28518965877367,11.1185348965652));
#14381=CARTESIAN_POINT('Ctrl Pts',(-3.50520498446835,1.2687667552278,11.1021119930194));
#14382=CARTESIAN_POINT('Ctrl Pts',(-3.50155748539241,1.25609154388858,11.0836597150224));
#14383=CARTESIAN_POINT('Ctrl Pts',(-3.49642218023894,1.23920409039234,11.0430495960472));
#14384=CARTESIAN_POINT('Ctrl Pts',(-3.495,1.235,11.0208800943307));
#14385=CARTESIAN_POINT('Ctrl Pts',(-3.495,1.235,10.9791199056693));
#14386=CARTESIAN_POINT('Ctrl Pts',(-3.49642218023894,1.23920409039234,10.9569504039528));
#14387=CARTESIAN_POINT('Ctrl Pts',(-3.50155748539241,1.25609154388858,10.9163402849776));
#14388=CARTESIAN_POINT('Ctrl Pts',(-3.50520498446835,1.2687667552278,10.8978880069806));
#14389=CARTESIAN_POINT('Ctrl Pts',(-3.50910475462832,1.28518965877367,10.8814651034348));
#14390=CARTESIAN_POINT('Ctrl Pts',(-3.50955146832001,1.28711294069536,10.8796310863737));
#14391=CARTESIAN_POINT('Ctrl Pts',(-3.51,1.28909463493591,10.8778320827713));
#14392=CARTESIAN_POINT('',(-3.51,1.4,11.165));
#14393=CARTESIAN_POINT('Origin',(-3.51,1.4,11.));
#14394=CARTESIAN_POINT('',(-3.11525427381648,1.4,11.165));
#14395=CARTESIAN_POINT('',(-3.51,1.4,11.165));
#14396=CARTESIAN_POINT('',(-3.11525427381648,1.4,10.835));
#14397=CARTESIAN_POINT('Ctrl Pts',(-3.11525427381648,1.4,10.835));
#14398=CARTESIAN_POINT('Ctrl Pts',(-3.11525427381648,1.37923124059256,10.835));
#14399=CARTESIAN_POINT('Ctrl Pts',(-3.11444724049474,1.35711110492666,10.8391602809924));
#14400=CARTESIAN_POINT('Ctrl Pts',(-3.11155135184996,1.31647293736623,10.8560135297833));
#14401=CARTESIAN_POINT('Ctrl Pts',(-3.10950639514836,1.29795075602263,10.8687040061858));
#14402=CARTESIAN_POINT('Ctrl Pts',(-3.10568276567606,1.26870458121656,10.8979501809919));
#14403=CARTESIAN_POINT('Ctrl Pts',(-3.10365291110046,1.25601365401642,10.9164726079093));
#14404=CARTESIAN_POINT('Ctrl Pts',(-3.10079172813942,1.23916007816136,10.9571116239066));
#14405=CARTESIAN_POINT('Ctrl Pts',(-3.1,1.235,10.9792320572765));
#14406=CARTESIAN_POINT('Ctrl Pts',(-3.1,1.235,11.0207679427235));
#14407=CARTESIAN_POINT('Ctrl Pts',(-3.10079172813942,1.23916007816136,11.0428883760934));
#14408=CARTESIAN_POINT('Ctrl Pts',(-3.10365291110046,1.25601365401642,11.0835273920907));
#14409=CARTESIAN_POINT('Ctrl Pts',(-3.10568276567606,1.26870458121656,11.1020498190081));
#14410=CARTESIAN_POINT('Ctrl Pts',(-3.10950639514836,1.29795075602263,11.1312959938142));
#14411=CARTESIAN_POINT('Ctrl Pts',(-3.11155135184996,1.31647293736623,11.1439864702167));
#14412=CARTESIAN_POINT('Ctrl Pts',(-3.11444724049474,1.35711110492666,11.1608397190076));
#14413=CARTESIAN_POINT('Ctrl Pts',(-3.11525427381648,1.37923124059256,11.165));
#14414=CARTESIAN_POINT('Ctrl Pts',(-3.11525427381648,1.4,11.165));
#14415=CARTESIAN_POINT('Ctrl Pts',(-3.11525427381648,1.4,11.165));
#14416=CARTESIAN_POINT('Ctrl Pts',(-3.11525427381648,1.42076875940744,11.165));
#14417=CARTESIAN_POINT('Ctrl Pts',(-3.11444724049474,1.44288889507334,11.1608397190076));
#14418=CARTESIAN_POINT('Ctrl Pts',(-3.11155135184996,1.48352706263377,11.1439864702167));
#14419=CARTESIAN_POINT('Ctrl Pts',(-3.10950639514836,1.50204924397737,11.1312959938142));
#14420=CARTESIAN_POINT('Ctrl Pts',(-3.10568276567606,1.53129541878343,11.1020498190081));
#14421=CARTESIAN_POINT('Ctrl Pts',(-3.10365291110046,1.54398634598358,11.0835273920907));
#14422=CARTESIAN_POINT('Ctrl Pts',(-3.10079172813942,1.56083992183864,11.0428883760934));
#14423=CARTESIAN_POINT('Ctrl Pts',(-3.1,1.565,11.0207679427235));
#14424=CARTESIAN_POINT('Ctrl Pts',(-3.1,1.565,10.9792320572765));
#14425=CARTESIAN_POINT('Ctrl Pts',(-3.10079172813942,1.56083992183864,10.9571116239066));
#14426=CARTESIAN_POINT('Ctrl Pts',(-3.10365291110046,1.54398634598358,10.9164726079093));
#14427=CARTESIAN_POINT('Ctrl Pts',(-3.10568276567606,1.53129541878343,10.8979501809919));
#14428=CARTESIAN_POINT('Ctrl Pts',(-3.10950639514836,1.50204924397737,10.8687040061858));
#14429=CARTESIAN_POINT('Ctrl Pts',(-3.11155135184996,1.48352706263377,10.8560135297833));
#14430=CARTESIAN_POINT('Ctrl Pts',(-3.11444724049474,1.44288889507334,10.8391602809924));
#14431=CARTESIAN_POINT('Ctrl Pts',(-3.11525427381648,1.42076875940744,10.835));
#14432=CARTESIAN_POINT('Ctrl Pts',(-3.11525427381648,1.4,10.835));
#14433=CARTESIAN_POINT('',(-3.51,1.51090536506409,11.1221679172287));
#14434=CARTESIAN_POINT('Origin',(-3.51,1.4,11.));
#14435=CARTESIAN_POINT('Ctrl Pts',(-3.51,1.51090536506409,10.8778320827713));
#14436=CARTESIAN_POINT('Ctrl Pts',(-3.50955146832001,1.51288705930464,10.8796310863737));
#14437=CARTESIAN_POINT('Ctrl Pts',(-3.50910475462832,1.51481034122633,10.8814651034348));
#14438=CARTESIAN_POINT('Ctrl Pts',(-3.50520498446835,1.5312332447722,10.8978880069806));
#14439=CARTESIAN_POINT('Ctrl Pts',(-3.50155748539241,1.54390845611142,10.9163402849776));
#14440=CARTESIAN_POINT('Ctrl Pts',(-3.49642218023894,1.56079590960766,10.9569504039528));
#14441=CARTESIAN_POINT('Ctrl Pts',(-3.495,1.565,10.9791199056693));
#14442=CARTESIAN_POINT('Ctrl Pts',(-3.495,1.565,11.0208800943307));
#14443=CARTESIAN_POINT('Ctrl Pts',(-3.49642218023894,1.56079590960766,11.0430495960472));
#14444=CARTESIAN_POINT('Ctrl Pts',(-3.50155748539241,1.54390845611142,11.0836597150224));
#14445=CARTESIAN_POINT('Ctrl Pts',(-3.50520498446835,1.5312332447722,11.1021119930194));
#14446=CARTESIAN_POINT('Ctrl Pts',(-3.50910475462832,1.51481034122633,11.1185348965652));
#14447=CARTESIAN_POINT('Ctrl Pts',(-3.50955146832001,1.51288705930464,11.1203689136263));
#14448=CARTESIAN_POINT('Ctrl Pts',(-3.51,1.51090536506409,11.1221679172287));
#14449=CARTESIAN_POINT('Origin',(-3.51,1.4,11.));
#14450=CARTESIAN_POINT('',(-3.51,1.,11.1221679172287));
#14451=CARTESIAN_POINT('Origin',(-4.,1.,11.));
#14452=CARTESIAN_POINT('',(-4.505,1.8,11.));
#14453=CARTESIAN_POINT('Origin',(-4.,1.8,11.));
#14454=CARTESIAN_POINT('',(-4.505,1.,11.));
#14455=CARTESIAN_POINT('',(-4.505,1.,11.));
#14456=CARTESIAN_POINT('Origin',(-4.,1.,11.));
#14457=CARTESIAN_POINT('Origin',(-4.,1.,11.));
#14458=CARTESIAN_POINT('',(-4.9,1.8,11.));
#14459=CARTESIAN_POINT('Origin',(-4.,1.8,11.));
#14460=CARTESIAN_POINT('',(-4.9,1.,11.));
#14461=CARTESIAN_POINT('',(-4.9,1.,11.));
#14462=CARTESIAN_POINT('Origin',(-4.,1.,11.));
#14463=CARTESIAN_POINT('Origin',(-4.,1.8,11.));
#14464=CARTESIAN_POINT('Origin',(-4.,1.,11.));
#14465=CARTESIAN_POINT('',(0.,0.,0.));
#14466=CARTESIAN_POINT('Origin',(-2.82632109303527,-4.2,8.79263101785268));
#14467=CARTESIAN_POINT('',(-2.99132109303527,-4.2,8.79263101785268));
#14468=CARTESIAN_POINT('Origin',(-2.82632109303527,-4.2,8.79263101785268));
#14469=CARTESIAN_POINT('',(-2.99132109303527,-2.7,8.79263101785268));
#14470=CARTESIAN_POINT('',(-2.99132109303527,-4.2,8.79263101785268));
#14471=CARTESIAN_POINT('Origin',(-2.82632109303527,-2.7,8.79263101785268));
#14472=CARTESIAN_POINT('Origin',(-2.82632109303527,-4.2,8.79263101785268));
#14473=CARTESIAN_POINT('Origin',(-2.82632109303527,-5.8,8.79263101785268));
#14474=CARTESIAN_POINT('',(-2.99132109303527,-5.7,8.79263101785268));
#14475=CARTESIAN_POINT('Origin',(-2.82632109303527,-5.7,8.79263101785268));
#14476=CARTESIAN_POINT('',(-2.99132109303527,-4.7,8.79263101785268));
#14477=CARTESIAN_POINT('',(-2.99132109303527,-5.8,8.79263101785268));
#14478=CARTESIAN_POINT('Origin',(-2.82632109303527,-4.7,8.79263101785268));
#14479=CARTESIAN_POINT('Origin',(-2.82632109303527,-4.7,8.79263101785268));
#14480=CARTESIAN_POINT('Origin',(-2.82632109303527,-3.5,8.79263101785268));
#14481=CARTESIAN_POINT('',(-3.52632109303527,-3.5,8.79263101785268));
#14482=CARTESIAN_POINT('Origin',(-2.82632109303527,-3.5,8.79263101785268));
#14483=CARTESIAN_POINT('',(-3.12632109303527,-3.5,8.79263101785268));
#14484=CARTESIAN_POINT('Origin',(-2.82632109303527,-3.5,8.79263101785268));
#14485=CARTESIAN_POINT('Origin',(-2.82632109303527,-3.9,8.79263101785268));
#14486=CARTESIAN_POINT('',(-3.52632109303527,-3.9,8.79263101785268));
#14487=CARTESIAN_POINT('Origin',(-2.82632109303527,-3.9,8.79263101785268));
#14488=CARTESIAN_POINT('',(-3.12632109303527,-3.9,8.79263101785268));
#14489=CARTESIAN_POINT('Origin',(-2.82632109303527,-3.9,8.79263101785268));
#14490=CARTESIAN_POINT('Origin',(-2.82632109303527,-3.9,8.79263101785268));
#14491=CARTESIAN_POINT('',(-3.52632109303527,-3.9,8.79263101785268));
#14492=CARTESIAN_POINT('Origin',(-2.82632109303527,-5.7,8.79263101785268));
#14493=CARTESIAN_POINT('',(-3.12632109303527,-5.7,8.79263101785268));
#14494=CARTESIAN_POINT('',(-3.12632109303527,-5.7,8.79263101785268));
#14495=CARTESIAN_POINT('Origin',(-2.82632109303527,-5.7,8.79263101785268));
#14496=CARTESIAN_POINT('Origin',(-2.82632109303527,-5.7,8.79263101785268));
#14497=CARTESIAN_POINT('',(-3.12632109303527,-2.7,8.79263101785268));
#14498=CARTESIAN_POINT('Origin',(-2.82632109303527,-2.7,8.79263101785268));
#14499=CARTESIAN_POINT('',(-3.12632109303527,-5.7,8.79263101785268));
#14500=CARTESIAN_POINT('Origin',(-2.82632109303527,-2.7,8.79263101785268));
#14501=CARTESIAN_POINT('Origin',(-2.82632109303527,-5.7,8.79263101785268));
#14502=CARTESIAN_POINT('',(0.,0.,0.));
#14503=CARTESIAN_POINT('Origin',(-2.82632109303527,-4.7,8.79263101785268));
#14504=CARTESIAN_POINT('',(-3.13132109303527,-3.9,8.79263101785268));
#14505=CARTESIAN_POINT('Origin',(-2.82632109303527,-3.9,8.79263101785268));
#14506=CARTESIAN_POINT('',(-3.13132109303527,-4.7,8.79263101785268));
#14507=CARTESIAN_POINT('',(-3.13132109303527,-4.7,8.79263101785268));
#14508=CARTESIAN_POINT('Origin',(-2.82632109303527,-4.7,8.79263101785268));
#14509=CARTESIAN_POINT('Origin',(-2.82632109303527,-4.7,8.79263101785268));
#14510=CARTESIAN_POINT('',(-3.32632109303527,-3.9,8.79263101785268));
#14511=CARTESIAN_POINT('Origin',(-2.82632109303527,-3.9,8.79263101785268));
#14512=CARTESIAN_POINT('',(-3.32632109303527,-4.7,8.79263101785268));
#14513=CARTESIAN_POINT('',(-3.32632109303527,-4.7,8.79263101785268));
#14514=CARTESIAN_POINT('Origin',(-2.82632109303527,-4.7,8.79263101785268));
#14515=CARTESIAN_POINT('Origin',(-2.82632109303527,-3.9,8.79263101785268));
#14516=CARTESIAN_POINT('Origin',(-2.82632109303527,-4.7,8.79263101785268));
#14517=CARTESIAN_POINT('',(0.,0.,0.));
#14518=CARTESIAN_POINT('Origin',(-2.82632109303527,-5.7,8.79263101785268));
#14519=CARTESIAN_POINT('',(-3.13132109303527,-5.5,8.79263101785268));
#14520=CARTESIAN_POINT('Origin',(-2.82632109303527,-5.5,8.79263101785268));
#14521=CARTESIAN_POINT('',(-3.13132109303527,-5.7,8.79263101785268));
#14522=CARTESIAN_POINT('',(-3.13132109303527,-5.7,8.79263101785268));
#14523=CARTESIAN_POINT('Origin',(-2.82632109303527,-5.7,8.79263101785268));
#14524=CARTESIAN_POINT('Origin',(-2.82632109303527,-5.7,8.79263101785268));
#14525=CARTESIAN_POINT('',(-3.32632109303527,-5.5,8.79263101785268));
#14526=CARTESIAN_POINT('Origin',(-2.82632109303527,-5.5,8.79263101785268));
#14527=CARTESIAN_POINT('',(-3.32632109303527,-5.7,8.79263101785268));
#14528=CARTESIAN_POINT('',(-3.32632109303527,-5.7,8.79263101785268));
#14529=CARTESIAN_POINT('Origin',(-2.82632109303527,-5.7,8.79263101785268));
#14530=CARTESIAN_POINT('Origin',(-2.82632109303527,-5.5,8.79263101785268));
#14531=CARTESIAN_POINT('Origin',(-2.82632109303527,-5.7,8.79263101785268));
#14532=CARTESIAN_POINT('',(0.,0.,0.));
#14533=CARTESIAN_POINT('Origin',(-2.82632109303527,-5.9,8.79263101785268));
#14534=CARTESIAN_POINT('',(-3.05132109303527,-5.7,8.79263101785268));
#14535=CARTESIAN_POINT('Origin',(-2.82632109303527,-5.7,8.79263101785268));
#14536=CARTESIAN_POINT('',(-3.05132109303527,-5.9,8.79263101785268));
#14537=CARTESIAN_POINT('',(-3.05132109303527,-5.9,8.79263101785268));
#14538=CARTESIAN_POINT('Origin',(-2.82632109303527,-5.9,8.79263101785268));
#14539=CARTESIAN_POINT('Origin',(-2.82632109303527,-5.9,8.79263101785268));
#14540=CARTESIAN_POINT('',(-3.32632109303527,-5.7,8.79263101785268));
#14541=CARTESIAN_POINT('Origin',(-2.82632109303527,-5.7,8.79263101785268));
#14542=CARTESIAN_POINT('',(-3.32632109303527,-5.9,8.79263101785268));
#14543=CARTESIAN_POINT('',(-3.32632109303527,-5.9,8.79263101785268));
#14544=CARTESIAN_POINT('Origin',(-2.82632109303527,-5.9,8.79263101785268));
#14545=CARTESIAN_POINT('Origin',(-2.82632109303527,-5.7,8.79263101785268));
#14546=CARTESIAN_POINT('Origin',(-2.82632109303527,-5.9,8.79263101785268));
#14547=CARTESIAN_POINT('',(0.,0.,0.));
#14548=CARTESIAN_POINT('Origin',(-2.82632109303527,-2.7,8.79263101785268));
#14549=CARTESIAN_POINT('',(-3.05132109303527,-2.5,8.79263101785268));
#14550=CARTESIAN_POINT('Origin',(-2.82632109303527,-2.5,8.79263101785268));
#14551=CARTESIAN_POINT('',(-3.05132109303527,-2.7,8.79263101785268));
#14552=CARTESIAN_POINT('',(-3.05132109303527,-2.7,8.79263101785268));
#14553=CARTESIAN_POINT('Origin',(-2.82632109303527,-2.7,8.79263101785268));
#14554=CARTESIAN_POINT('Origin',(-2.82632109303527,-2.7,8.79263101785268));
#14555=CARTESIAN_POINT('',(-3.32632109303527,-2.5,8.79263101785268));
#14556=CARTESIAN_POINT('Origin',(-2.82632109303527,-2.5,8.79263101785268));
#14557=CARTESIAN_POINT('',(-3.32632109303527,-2.7,8.79263101785268));
#14558=CARTESIAN_POINT('',(-3.32632109303527,-2.7,8.79263101785268));
#14559=CARTESIAN_POINT('Origin',(-2.82632109303527,-2.7,8.79263101785268));
#14560=CARTESIAN_POINT('Origin',(-2.82632109303527,-2.5,8.79263101785268));
#14561=CARTESIAN_POINT('Origin',(-2.82632109303527,-2.7,8.79263101785268));
#14562=CARTESIAN_POINT('',(0.,0.,0.));
#14563=CARTESIAN_POINT('Origin',(0.,-0.4,0.));
#14564=CARTESIAN_POINT('',(-0.1954,-0.4,2.39295984553393E-17));
#14565=CARTESIAN_POINT('Origin',(0.,-0.4,0.));
#14566=CARTESIAN_POINT('Origin',(0.0577350269189626,0.,-0.1));
#14567=CARTESIAN_POINT('',(0.0577350269189626,0.,-0.1));
#14568=CARTESIAN_POINT('',(0.115470053837925,0.,0.));
#14569=CARTESIAN_POINT('',(0.0934187836487032,0.,-0.0381939203391614));
#14570=CARTESIAN_POINT('',(0.0577350269189626,-0.2,-0.1));
#14571=CARTESIAN_POINT('',(0.0577350269189626,0.,-0.1));
#14572=CARTESIAN_POINT('',(0.115470053837925,-0.2,0.));
#14573=CARTESIAN_POINT('',(0.115470053837925,-0.2,0.));
#14574=CARTESIAN_POINT('',(0.115470053837925,0.,0.));
#14575=CARTESIAN_POINT('Origin',(-0.0577350269189626,0.,-0.1));
#14576=CARTESIAN_POINT('',(-0.0577350269189626,0.,-0.1));
#14577=CARTESIAN_POINT('',(0.0561324865405187,0.,-0.1));
#14578=CARTESIAN_POINT('',(-0.0577350269189626,-0.2,-0.1));
#14579=CARTESIAN_POINT('',(-0.0577350269189626,0.,-0.1));
#14580=CARTESIAN_POINT('',(0.0577350269189626,-0.2,-0.1));
#14581=CARTESIAN_POINT('Origin',(-0.115470053837925,0.,-1.38777878078145E-17));
#14582=CARTESIAN_POINT('',(-0.115470053837925,0.,-1.41410031829988E-17));
#14583=CARTESIAN_POINT('',(-0.0797862971081845,0.,-0.0618060796608387));
#14584=CARTESIAN_POINT('',(-0.115470053837925,-0.2,-1.38777878078145E-17));
#14585=CARTESIAN_POINT('',(-0.115470053837925,0.,-1.41410031829988E-17));
#14586=CARTESIAN_POINT('',(-0.0577350269189626,-0.2,-0.1));
#14587=CARTESIAN_POINT('Origin',(-0.0577350269189626,0.,0.1));
#14588=CARTESIAN_POINT('',(-0.0577350269189626,0.,0.1));
#14589=CARTESIAN_POINT('',(-0.0509187836487033,0.,0.111806079660839));
#14590=CARTESIAN_POINT('',(-0.0577350269189626,-0.2,0.1));
#14591=CARTESIAN_POINT('',(-0.0577350269189626,0.,0.1));
#14592=CARTESIAN_POINT('',(-0.115470053837925,-0.2,-1.41410031829988E-17));
#14593=CARTESIAN_POINT('Origin',(0.0577350269189626,0.,0.1));
#14594=CARTESIAN_POINT('',(0.0577350269189626,0.,0.1));
#14595=CARTESIAN_POINT('',(0.113867513459481,0.,0.1));
#14596=CARTESIAN_POINT('',(0.0577350269189626,-0.2,0.1));
#14597=CARTESIAN_POINT('',(0.0577350269189626,0.,0.1));
#14598=CARTESIAN_POINT('',(-0.0577350269189626,-0.2,0.1));
#14599=CARTESIAN_POINT('Origin',(0.115470053837925,0.,0.));
#14600=CARTESIAN_POINT('',(0.122286297108185,0.,-0.0118060796608386));
#14601=CARTESIAN_POINT('',(0.0577350269189626,-0.2,0.1));
#14602=CARTESIAN_POINT('Origin',(0.,-0.2,0.));
#14603=CARTESIAN_POINT('Origin',(0.17,0.,0.));
#14604=CARTESIAN_POINT('',(-0.17,-8.67361737988404E-18,-2.0818995585505E-17));
#14605=CARTESIAN_POINT('Origin',(0.,0.,0.));
#14606=CARTESIAN_POINT('Origin',(0.,-0.015,0.));
#14607=CARTESIAN_POINT('',(-0.1954,-0.0254,-2.39295984553393E-17));
#14608=CARTESIAN_POINT('Origin',(0.,-0.0254,0.));
#14609=CARTESIAN_POINT('',(-0.185,-0.015,-2.2655965784226E-17));
#14610=CARTESIAN_POINT('Origin',(0.,-0.2775,0.));
#14611=CARTESIAN_POINT('',(-0.1954,-0.2775,-2.39295984553393E-17));
#14612=CARTESIAN_POINT('',(0.,0.,0.));
#14613=CARTESIAN_POINT('Origin',(0.0866025403784439,-0.4,-0.15));
#14614=CARTESIAN_POINT('',(0.173205080756888,-0.4,0.));
#14615=CARTESIAN_POINT('',(0.0866025403784439,-0.4,-0.15));
#14616=CARTESIAN_POINT('',(0.173205080756888,-0.4,0.));
#14617=CARTESIAN_POINT('',(0.0866025403784439,-0.64,-0.15));
#14618=CARTESIAN_POINT('',(0.0866025403784439,-0.4,-0.15));
#14619=CARTESIAN_POINT('',(0.173205080756888,-0.64,0.));
#14620=CARTESIAN_POINT('',(0.173205080756888,-0.64,0.));
#14621=CARTESIAN_POINT('',(0.173205080756888,-0.4,0.));
#14622=CARTESIAN_POINT('Origin',(-0.0866025403784438,-0.4,-0.15));
#14623=CARTESIAN_POINT('',(-0.0866025403784438,-0.4,-0.15));
#14624=CARTESIAN_POINT('',(0.0866025403784439,-0.4,-0.15));
#14625=CARTESIAN_POINT('',(-0.0866025403784438,-0.64,-0.15));
#14626=CARTESIAN_POINT('',(-0.0866025403784438,-0.4,-0.15));
#14627=CARTESIAN_POINT('',(0.0866025403784439,-0.64,-0.15));
#14628=CARTESIAN_POINT('Origin',(-0.173205080756888,-0.4,-2.77555756156289E-17));
#14629=CARTESIAN_POINT('',(-0.173205080756888,-0.4,-2.12115047744981E-17));
#14630=CARTESIAN_POINT('',(-0.0866025403784438,-0.4,-0.15));
#14631=CARTESIAN_POINT('',(-0.173205080756888,-0.64,-2.77555756156289E-17));
#14632=CARTESIAN_POINT('',(-0.173205080756888,-0.4,-2.12115047744981E-17));
#14633=CARTESIAN_POINT('',(-0.0866025403784438,-0.64,-0.15));
#14634=CARTESIAN_POINT('Origin',(-0.0866025403784439,-0.4,0.15));
#14635=CARTESIAN_POINT('',(-0.0866025403784439,-0.4,0.15));
#14636=CARTESIAN_POINT('',(-0.173205080756888,-0.4,-2.12115047744981E-17));
#14637=CARTESIAN_POINT('',(-0.0866025403784439,-0.64,0.15));
#14638=CARTESIAN_POINT('',(-0.0866025403784439,-0.4,0.15));
#14639=CARTESIAN_POINT('',(-0.173205080756888,-0.64,-2.12115047744981E-17));
#14640=CARTESIAN_POINT('Origin',(0.0866025403784439,-0.4,0.15));
#14641=CARTESIAN_POINT('',(0.0866025403784439,-0.4,0.15));
#14642=CARTESIAN_POINT('',(-0.0866025403784439,-0.4,0.15));
#14643=CARTESIAN_POINT('',(0.0866025403784439,-0.64,0.15));
#14644=CARTESIAN_POINT('',(0.0866025403784439,-0.4,0.15));
#14645=CARTESIAN_POINT('',(-0.0866025403784439,-0.64,0.15));
#14646=CARTESIAN_POINT('Origin',(0.173205080756888,-0.4,0.));
#14647=CARTESIAN_POINT('',(0.0866025403784439,-0.4,0.15));
#14648=CARTESIAN_POINT('',(0.0866025403784439,-0.64,0.15));
#14649=CARTESIAN_POINT('Origin',(0.,-0.4,-2.77555756156289E-17));
#14650=CARTESIAN_POINT('Origin',(0.,-0.64,-2.77555756156289E-17));
#14651=CARTESIAN_POINT('Origin',(0.,-1.,0.));
#14652=CARTESIAN_POINT('',(-0.1954,-1.,2.39295984553393E-17));
#14653=CARTESIAN_POINT('Origin',(0.,-1.,0.));
#14654=CARTESIAN_POINT('Origin',(0.3,0.4,0.));
#14655=CARTESIAN_POINT('',(-0.3,0.4,-3.67394039744206E-17));
#14656=CARTESIAN_POINT('Origin',(0.,0.4,0.));
#14657=CARTESIAN_POINT('Origin',(0.,0.375,0.));
#14658=CARTESIAN_POINT('',(-0.35,0.35,-4.28626379701573E-17));
#14659=CARTESIAN_POINT('Origin',(0.,0.35,0.));
#14660=CARTESIAN_POINT('',(-0.325,0.375,-3.9801020972289E-17));
#14661=CARTESIAN_POINT('Origin',(0.,0.19,0.));
#14662=CARTESIAN_POINT('',(-0.35,0.03,-4.28626379701574E-17));
#14663=CARTESIAN_POINT('Origin',(0.,0.03,0.));
#14664=CARTESIAN_POINT('',(-0.35,0.19,-4.28626379701574E-17));
#14665=CARTESIAN_POINT('Origin',(0.,0.0149999999999999,0.));
#14666=CARTESIAN_POINT('',(-0.32,-3.29597460435593E-17,-3.91886975727153E-17));
#14667=CARTESIAN_POINT('Origin',(0.,0.,0.));
#14668=CARTESIAN_POINT('',(-0.335,0.0149999999999999,-4.10256677714363E-17));
#14669=CARTESIAN_POINT('Origin',(0.22,0.,0.));
#14670=CARTESIAN_POINT('',(-0.22,-6.93889390390723E-18,-2.69422295812418E-17));
#14671=CARTESIAN_POINT('Origin',(0.,0.,0.));
#14672=CARTESIAN_POINT('Origin',(0.,-0.02,0.));
#14673=CARTESIAN_POINT('',(-0.1954,-0.0492,2.39295984553393E-17));
#14674=CARTESIAN_POINT('Origin',(0.,-0.0492,0.));
#14675=CARTESIAN_POINT('',(-0.21,-0.02,-2.57175827820944E-17));
#14676=CARTESIAN_POINT('Origin',(0.,-0.8,0.));
#14677=CARTESIAN_POINT('',(-0.1954,-0.8,-2.39295984553393E-17));
#14678=CARTESIAN_POINT('',(0.,0.,0.));
#14679=CARTESIAN_POINT('Origin',(0.3,0.4,0.));
#14680=CARTESIAN_POINT('',(-0.3,0.4,-3.67394039744206E-17));
#14681=CARTESIAN_POINT('Origin',(0.,0.4,0.));
#14682=CARTESIAN_POINT('Origin',(0.,0.375,0.));
#14683=CARTESIAN_POINT('',(-0.35,0.35,-4.28626379701573E-17));
#14684=CARTESIAN_POINT('Origin',(0.,0.35,0.));
#14685=CARTESIAN_POINT('',(-0.325,0.375,-3.9801020972289E-17));
#14686=CARTESIAN_POINT('Origin',(0.,0.19,0.));
#14687=CARTESIAN_POINT('',(-0.35,0.03,-4.28626379701574E-17));
#14688=CARTESIAN_POINT('Origin',(0.,0.03,0.));
#14689=CARTESIAN_POINT('',(-0.35,0.19,-4.28626379701574E-17));
#14690=CARTESIAN_POINT('Origin',(0.,0.0149999999999999,0.));
#14691=CARTESIAN_POINT('',(-0.32,-3.29597460435593E-17,-3.91886975727153E-17));
#14692=CARTESIAN_POINT('Origin',(0.,0.,0.));
#14693=CARTESIAN_POINT('',(-0.335,0.0149999999999999,-4.10256677714363E-17));
#14694=CARTESIAN_POINT('Origin',(0.22,0.,0.));
#14695=CARTESIAN_POINT('',(-0.22,-6.93889390390723E-18,-2.69422295812418E-17));
#14696=CARTESIAN_POINT('Origin',(0.,0.,0.));
#14697=CARTESIAN_POINT('Origin',(0.,-0.02,0.));
#14698=CARTESIAN_POINT('',(-0.1954,-0.0492,2.39295984553393E-17));
#14699=CARTESIAN_POINT('Origin',(0.,-0.0492,0.));
#14700=CARTESIAN_POINT('',(-0.21,-0.02,-2.57175827820944E-17));
#14701=CARTESIAN_POINT('Origin',(0.,-0.8,0.));
#14702=CARTESIAN_POINT('',(-0.1954,-1.5646,2.39295984553393E-17));
#14703=CARTESIAN_POINT('Origin',(0.,-1.5646,0.));
#14704=CARTESIAN_POINT('',(-0.1954,-0.8,-2.39295984553393E-17));
#14705=CARTESIAN_POINT('Origin',(0.,-1.58,0.));
#14706=CARTESIAN_POINT('',(-0.16,-1.6,-1.95943487863577E-17));
#14707=CARTESIAN_POINT('Origin',(0.,-1.6,0.));
#14708=CARTESIAN_POINT('',(-0.18,-1.58,-2.20436423846524E-17));
#14709=CARTESIAN_POINT('Origin',(0.,-1.6,0.));
#14710=CARTESIAN_POINT('Origin',(0.0866025403784439,-0.4,-0.15));
#14711=CARTESIAN_POINT('',(0.173205080756888,-0.4,0.));
#14712=CARTESIAN_POINT('',(0.0866025403784439,-0.4,-0.15));
#14713=CARTESIAN_POINT('',(0.173205080756888,-0.4,0.));
#14714=CARTESIAN_POINT('',(0.0866025403784439,-0.64,-0.15));
#14715=CARTESIAN_POINT('',(0.0866025403784439,-0.4,-0.15));
#14716=CARTESIAN_POINT('',(0.173205080756888,-0.64,0.));
#14717=CARTESIAN_POINT('',(0.173205080756888,-0.64,0.));
#14718=CARTESIAN_POINT('',(0.173205080756888,-0.4,0.));
#14719=CARTESIAN_POINT('Origin',(-0.0866025403784438,-0.4,-0.15));
#14720=CARTESIAN_POINT('',(-0.0866025403784438,-0.4,-0.15));
#14721=CARTESIAN_POINT('',(0.0866025403784439,-0.4,-0.15));
#14722=CARTESIAN_POINT('',(-0.0866025403784438,-0.64,-0.15));
#14723=CARTESIAN_POINT('',(-0.0866025403784438,-0.4,-0.15));
#14724=CARTESIAN_POINT('',(0.0866025403784439,-0.64,-0.15));
#14725=CARTESIAN_POINT('Origin',(-0.173205080756888,-0.4,-2.77555756156289E-17));
#14726=CARTESIAN_POINT('',(-0.173205080756888,-0.4,-2.12115047744981E-17));
#14727=CARTESIAN_POINT('',(-0.0866025403784438,-0.4,-0.15));
#14728=CARTESIAN_POINT('',(-0.173205080756888,-0.64,-2.77555756156289E-17));
#14729=CARTESIAN_POINT('',(-0.173205080756888,-0.4,-2.12115047744981E-17));
#14730=CARTESIAN_POINT('',(-0.0866025403784438,-0.64,-0.15));
#14731=CARTESIAN_POINT('Origin',(-0.0866025403784439,-0.4,0.15));
#14732=CARTESIAN_POINT('',(-0.0866025403784439,-0.4,0.15));
#14733=CARTESIAN_POINT('',(-0.173205080756888,-0.4,-2.12115047744981E-17));
#14734=CARTESIAN_POINT('',(-0.0866025403784439,-0.64,0.15));
#14735=CARTESIAN_POINT('',(-0.0866025403784439,-0.4,0.15));
#14736=CARTESIAN_POINT('',(-0.173205080756888,-0.64,-2.12115047744981E-17));
#14737=CARTESIAN_POINT('Origin',(0.0866025403784439,-0.4,0.15));
#14738=CARTESIAN_POINT('',(0.0866025403784439,-0.4,0.15));
#14739=CARTESIAN_POINT('',(-0.0866025403784439,-0.4,0.15));
#14740=CARTESIAN_POINT('',(0.0866025403784439,-0.64,0.15));
#14741=CARTESIAN_POINT('',(0.0866025403784439,-0.4,0.15));
#14742=CARTESIAN_POINT('',(-0.0866025403784439,-0.64,0.15));
#14743=CARTESIAN_POINT('Origin',(0.173205080756888,-0.4,0.));
#14744=CARTESIAN_POINT('',(0.0866025403784439,-0.4,0.15));
#14745=CARTESIAN_POINT('',(0.0866025403784439,-0.64,0.15));
#14746=CARTESIAN_POINT('Origin',(0.,-0.4,-2.77555756156289E-17));
#14747=CARTESIAN_POINT('Origin',(0.,-0.64,-2.77555756156289E-17));
#14748=CARTESIAN_POINT('',(0.,0.,0.));
#14749=CARTESIAN_POINT('',(0.,0.,0.));
#14750=CARTESIAN_POINT('',(0.,0.,0.));
#14751=CARTESIAN_POINT('',(0.,0.,0.));
#14752=CARTESIAN_POINT('',(0.,0.,0.));
#14753=CARTESIAN_POINT('',(0.,0.,0.));
#14754=CARTESIAN_POINT('',(0.,0.,0.));
#14755=CARTESIAN_POINT('',(0.,0.,0.));
#14756=CARTESIAN_POINT('',(0.,0.,0.));
#14757=CARTESIAN_POINT('',(0.,0.,0.));
#14758=CARTESIAN_POINT('',(0.,0.,0.));
#14759=CARTESIAN_POINT('',(0.,0.,0.));
#14760=CARTESIAN_POINT('',(-9.5,-6.,-1.));
#14761=CARTESIAN_POINT('',(-4.5,-6.,-0.58));
#14762=CARTESIAN_POINT('',(-4.5,-6.,1.));
#14763=CARTESIAN_POINT('',(-4.5,-6.,-1.42));
#14764=CARTESIAN_POINT('',(-4.5,-6.,-2.8));
#14765=CARTESIAN_POINT('',(-4.5,-6.,-2.9));
#14766=CARTESIAN_POINT('',(2.5,-6.,-0.58));
#14767=CARTESIAN_POINT('',(2.5,-6.,1.));
#14768=CARTESIAN_POINT('',(2.5,-6.,-1.42));
#14769=CARTESIAN_POINT('',(2.5,-6.,-2.8));
#14770=CARTESIAN_POINT('',(2.5,-6.,-2.9));
#14771=CARTESIAN_POINT('',(-9.5,4.,-1.));
#14772=CARTESIAN_POINT('',(-4.5,4.,-0.58));
#14773=CARTESIAN_POINT('',(-4.5,4.,1.));
#14774=CARTESIAN_POINT('',(-4.5,4.,-1.42));
#14775=CARTESIAN_POINT('',(-4.5,4.,-2.8));
#14776=CARTESIAN_POINT('',(-4.5,4.,-2.9));
#14777=CARTESIAN_POINT('',(2.5,4.,-0.58));
#14778=CARTESIAN_POINT('',(2.5,4.,1.));
#14779=CARTESIAN_POINT('',(2.5,4.,-1.42));
#14780=CARTESIAN_POINT('',(2.5,4.,-2.8));
#14781=CARTESIAN_POINT('',(2.5,4.,-2.9));
#14782=CARTESIAN_POINT('',(-8.5,-1.4,1.8));
#14783=CARTESIAN_POINT('',(-8.5,1.4,1.8));
#14784=CARTESIAN_POINT('',(-6.,-1.4,1.8));
#14785=CARTESIAN_POINT('',(-6.,1.4,1.8));
#14786=CARTESIAN_POINT('',(-4.,0.,11.));
#14787=CARTESIAN_POINT('',(0.,0.,14.));
#14788=CARTESIAN_POINT('',(-2.76256313292354,-1.,12.2374368670765));
#14789=CARTESIAN_POINT('',(-5.23743686707646,-1.,12.2374368670765));
#14790=CARTESIAN_POINT('',(-5.23743686707646,-1.,9.76256313292354));
#14791=CARTESIAN_POINT('',(-2.76256313292354,-1.,9.76256313292354));
#14792=CARTESIAN_POINT('',(-2.76256313292354,1.,12.2374368670765));
#14793=CARTESIAN_POINT('',(-5.23743686707646,1.,12.2374368670765));
#14794=CARTESIAN_POINT('',(-5.23743686707646,1.,9.76256313292354));
#14795=CARTESIAN_POINT('',(-2.76256313292354,1.,9.76256313292354));
#14796=CARTESIAN_POINT('',(1.13137084989848,1.13137084989848,16.9));
#14797=CARTESIAN_POINT('',(-1.13137084989848,1.13137084989848,16.9));
#14798=CARTESIAN_POINT('',(-1.13137084989848,-1.13137084989848,16.9));
#14799=CARTESIAN_POINT('',(1.13137084989848,-1.13137084989848,16.9));
#14800=CARTESIAN_POINT('',(-1.5,-4.5,0.));
#14801=CARTESIAN_POINT('',(-1.5,2.,0.));
#14802=CARTESIAN_POINT('',(1.5,-4.5,0.));
#14803=CARTESIAN_POINT('',(1.5,2.,0.));
#14804=CARTESIAN_POINT('',(-5.25982293614231,0.8,14.8604204653858));
#14805=CARTESIAN_POINT('',(0.,0.,0.));
#14806=CARTESIAN_POINT('',(0.,0.,0.));
#14807=CARTESIAN_POINT('',(0.,0.,0.));
#14808=CARTESIAN_POINT('',(0.,0.,0.));
#14809=CARTESIAN_POINT('',(0.,0.,0.));
#14810=CARTESIAN_POINT('',(0.,0.,0.));
#14811=CARTESIAN_POINT('',(0.,0.,0.));
#14812=CARTESIAN_POINT('',(0.,0.,0.));
#14813=CARTESIAN_POINT('',(-3.1,1.4,11.));
#14814=CARTESIAN_POINT('',(-2.82632109303527,-5.9,8.79263101785268));
#14815=CARTESIAN_POINT('',(-2.82632109303527,-2.5,8.79263101785268));
#14816=CARTESIAN_POINT('',(0.,0.,0.));
#14817=CARTESIAN_POINT('',(0.,0.,0.));
#14818=CARTESIAN_POINT('Origin',(-2.82632109303527,-5.6,8.79263101785268));
#14819=CARTESIAN_POINT('',(-3.32632109303527,-5.5,8.79263101785268));
#14820=CARTESIAN_POINT('Origin',(-2.82632109303527,-5.5,8.79263101785268));
#14821=CARTESIAN_POINT('',(-3.32632109303527,-4.7,8.79263101785268));
#14822=CARTESIAN_POINT('',(-3.32632109303527,-5.6,8.79263101785268));
#14823=CARTESIAN_POINT('Origin',(-2.82632109303527,-4.7,8.79263101785268));
#14824=CARTESIAN_POINT('Origin',(0.,-5.6,4.668081457105));
#14825=CARTESIAN_POINT('',(-0.5,-5.5,4.668081457105));
#14826=CARTESIAN_POINT('Origin',(0.,-5.5,4.668081457105));
#14827=CARTESIAN_POINT('',(-0.5,-4.7,4.668081457105));
#14828=CARTESIAN_POINT('',(-0.5,-5.6,4.668081457105));
#14829=CARTESIAN_POINT('Origin',(0.,-4.7,4.668081457105));
#14830=CARTESIAN_POINT('Origin',(0.,-5.5,4.668081457105));
#14831=CARTESIAN_POINT('',(-0.765462347451497,-4.7,4.90060542282476));
#14832=CARTESIAN_POINT('',(-0.765462347451497,-5.5,4.90060542282476));
#14833=CARTESIAN_POINT('',(-0.765462347451497,-5.5,4.90060542282476));
#14834=CARTESIAN_POINT('',(0.059447564698039,-4.7,5.46586964143181));
#14835=CARTESIAN_POINT('Origin',(0.,-4.7,4.668081457105));
#14836=CARTESIAN_POINT('',(0.059447564698039,-5.5,5.46586964143181));
#14837=CARTESIAN_POINT('',(0.059447564698039,-5.5,5.46586964143181));
#14838=CARTESIAN_POINT('Origin',(0.,-5.5,4.668081457105));
#14839=CARTESIAN_POINT('Origin',(-0.412454956074768,-5.5,4.38544934780147));
#14840=CARTESIAN_POINT('',(-2.88576865773331,-5.5,7.99484283352587));
#14841=CARTESIAN_POINT('',(-0.412454956074768,-5.5,4.38544934780147));
#14842=CARTESIAN_POINT('',(-2.88576865773331,-4.7,7.99484283352587));
#14843=CARTESIAN_POINT('',(-2.88576865773331,-5.5,7.99484283352587));
#14844=CARTESIAN_POINT('',(-0.412454956074768,-4.7,4.38544934780147));
#14845=CARTESIAN_POINT('Origin',(-2.82632109303527,-5.5,8.79263101785268));
#14846=CARTESIAN_POINT('',(-2.06085874558378,-5.5,8.56010705213293));
#14847=CARTESIAN_POINT('',(-2.4138661369605,-5.5,9.07526312715621));
#14848=CARTESIAN_POINT('Origin',(-2.82632109303527,-5.5,8.79263101785268));
#14849=CARTESIAN_POINT('Origin',(-2.4138661369605,-5.5,9.07526312715621));
#14850=CARTESIAN_POINT('',(-2.06085874558378,-4.7,8.56010705213293));
#14851=CARTESIAN_POINT('',(-2.4138661369605,-4.7,9.07526312715621));
#14852=CARTESIAN_POINT('',(-2.06085874558378,-5.5,8.56010705213293));
#14853=CARTESIAN_POINT('Origin',(-2.82632109303527,-5.5,8.79263101785268));
#14854=CARTESIAN_POINT('Origin',(-2.82632109303527,-4.7,8.79263101785268));
#14855=CARTESIAN_POINT('Origin',(-2.82632109303527,-4.7,8.79263101785268));
#14856=CARTESIAN_POINT('',(0.,0.,0.));
#14857=CARTESIAN_POINT('Origin',(-2.82632109303527,-5.5,8.79263101785268));
#14858=CARTESIAN_POINT('',(-3.13132109303527,-4.7,8.79263101785268));
#14859=CARTESIAN_POINT('Origin',(-2.82632109303527,-4.7,8.79263101785268));
#14860=CARTESIAN_POINT('',(-3.13132109303527,-5.5,8.79263101785268));
#14861=CARTESIAN_POINT('',(-3.13132109303527,-5.5,8.79263101785268));
#14862=CARTESIAN_POINT('Origin',(-2.82632109303527,-5.5,8.79263101785268));
#14863=CARTESIAN_POINT('Origin',(-2.82632109303527,-5.5,8.79263101785268));
#14864=CARTESIAN_POINT('',(-3.32632109303527,-4.7,8.79263101785268));
#14865=CARTESIAN_POINT('Origin',(-2.82632109303527,-4.7,8.79263101785268));
#14866=CARTESIAN_POINT('',(-3.32632109303527,-5.5,8.79263101785268));
#14867=CARTESIAN_POINT('',(-3.32632109303527,-5.5,8.79263101785268));
#14868=CARTESIAN_POINT('Origin',(-2.82632109303527,-5.5,8.79263101785268));
#14869=CARTESIAN_POINT('Origin',(-2.82632109303527,-4.7,8.79263101785268));
#14870=CARTESIAN_POINT('Origin',(-2.82632109303527,-5.5,8.79263101785268));
#14871=CARTESIAN_POINT('',(0.,0.,0.));
#14872=CARTESIAN_POINT('Origin',(0.,-5.5,4.668081457105));
#14873=CARTESIAN_POINT('',(-0.305,-4.7,4.668081457105));
#14874=CARTESIAN_POINT('Origin',(0.,-4.7,4.668081457105));
#14875=CARTESIAN_POINT('',(-0.305,-5.5,4.668081457105));
#14876=CARTESIAN_POINT('',(-0.305,-5.5,4.668081457105));
#14877=CARTESIAN_POINT('Origin',(0.,-5.5,4.668081457105));
#14878=CARTESIAN_POINT('Origin',(0.,-5.5,4.668081457105));
#14879=CARTESIAN_POINT('',(-0.5,-4.7,4.668081457105));
#14880=CARTESIAN_POINT('Origin',(0.,-4.7,4.668081457105));
#14881=CARTESIAN_POINT('',(-0.5,-5.5,4.668081457105));
#14882=CARTESIAN_POINT('',(-0.5,-5.5,4.668081457105));
#14883=CARTESIAN_POINT('Origin',(0.,-5.5,4.668081457105));
#14884=CARTESIAN_POINT('Origin',(0.,-4.7,4.668081457105));
#14885=CARTESIAN_POINT('Origin',(0.,-5.5,4.668081457105));
#14886=CARTESIAN_POINT('',(0.,0.,0.));
#14887=CARTESIAN_POINT('',(0.,0.,0.));
#14888=CARTESIAN_POINT('',(0.,0.,0.));
#14889=CARTESIAN_POINT('',(0.,0.,0.));
#14890=CARTESIAN_POINT('',(0.,0.,0.));
#14891=CARTESIAN_POINT('Origin',(0.,-6.1,4.668081457105));
#14892=CARTESIAN_POINT('',(-0.305,-4.69,4.668081457105));
#14893=CARTESIAN_POINT('Origin',(0.,-4.69,4.668081457105));
#14894=CARTESIAN_POINT('',(-0.305,-3.8,4.668081457105));
#14895=CARTESIAN_POINT('',(-0.305,-6.1,4.668081457105));
#14896=CARTESIAN_POINT('Origin',(0.,-3.8,4.668081457105));
#14897=CARTESIAN_POINT('Origin',(0.,-3.8,4.668081457105));
#14898=CARTESIAN_POINT('Origin',(0.,-4.69,4.668081457105));
#14899=CARTESIAN_POINT('',(-0.8,-4.69,4.16808146));
#14900=CARTESIAN_POINT('',(-0.8,-4.69,5.16808146));
#14901=CARTESIAN_POINT('',(-0.8,-4.69,4.4180814585525));
#14902=CARTESIAN_POINT('',(0.8,-4.69,4.16808146));
#14903=CARTESIAN_POINT('',(0.,-4.69,4.16808146));
#14904=CARTESIAN_POINT('',(0.8,-4.69,5.16808146));
#14905=CARTESIAN_POINT('',(0.8,-4.69,4.4180814585525));
#14906=CARTESIAN_POINT('',(0.,-4.69,5.16808146));
#14907=CARTESIAN_POINT('Origin',(0.8,-6.,4.16808146));
#14908=CARTESIAN_POINT('',(0.8,-0.894427190999916,4.16808146));
#14909=CARTESIAN_POINT('',(0.8,-6.,4.16808146));
#14910=CARTESIAN_POINT('',(0.8,-0.894427190999916,4.36808146));
#14911=CARTESIAN_POINT('',(0.8,-0.894427190999916,3.4));
#14912=CARTESIAN_POINT('',(0.8,0.,4.36808146));
#14913=CARTESIAN_POINT('',(0.8,-3.,4.36808146));
#14914=CARTESIAN_POINT('',(0.8,0.,5.16808146));
#14915=CARTESIAN_POINT('',(0.8,0.,4.16808146));
#14916=CARTESIAN_POINT('',(0.8,-6.,5.16808146));
#14917=CARTESIAN_POINT('Origin',(0.,-3.,4.16808146));
#14918=CARTESIAN_POINT('',(-0.8,-0.894427190999916,4.16808146));
#14919=CARTESIAN_POINT('',(-0.8,0.,4.16808146));
#14920=CARTESIAN_POINT('Origin',(0.,0.,4.16808146));
#14921=CARTESIAN_POINT('Origin',(-0.8,0.,4.16808146));
#14922=CARTESIAN_POINT('',(-0.8,0.,5.16808146));
#14923=CARTESIAN_POINT('',(-0.8,0.,5.16808146));
#14924=CARTESIAN_POINT('',(-0.8,0.,4.36808146));
#14925=CARTESIAN_POINT('',(-0.8,0.,4.16808146));
#14926=CARTESIAN_POINT('',(-0.8,-0.894427190999916,4.36808146));
#14927=CARTESIAN_POINT('',(-0.8,0.,4.36808146));
#14928=CARTESIAN_POINT('',(-0.8,-0.894427190999916,3.4));
#14929=CARTESIAN_POINT('Origin',(0.8,0.,4.16808146));
#14930=CARTESIAN_POINT('',(0.6,0.,5.16808146));
#14931=CARTESIAN_POINT('',(0.6,0.,4.36808146));
#14932=CARTESIAN_POINT('',(0.6,0.,4.36808146));
#14933=CARTESIAN_POINT('',(0.8,0.,5.16808146));
#14934=CARTESIAN_POINT('',(0.4,0.,4.36808146));
#14935=CARTESIAN_POINT('Origin',(0.8,0.,4.16808146));
#14936=CARTESIAN_POINT('',(-0.6,-7.34788079488412E-17,4.36808146));
#14937=CARTESIAN_POINT('',(0.4,0.,4.36808146));
#14938=CARTESIAN_POINT('',(-0.6,0.,5.16808146));
#14939=CARTESIAN_POINT('',(0.8,0.,5.16808146));
#14940=CARTESIAN_POINT('',(-0.6,0.,4.36808146));
#14941=CARTESIAN_POINT('Origin',(0.,-3.,5.16808146));
#14942=CARTESIAN_POINT('Origin',(0.,0.,5.16808146));
#14943=CARTESIAN_POINT('Origin',(0.,0.,4.36808146));
#14944=CARTESIAN_POINT('',(-0.6,-7.34788079488412E-17,19.));
#14945=CARTESIAN_POINT('Origin',(0.,0.,19.));
#14946=CARTESIAN_POINT('',(-0.6,-7.34788079488412E-17,4.36808146));
#14947=CARTESIAN_POINT('Origin',(0.,0.,4.36808146));
#14948=CARTESIAN_POINT('Origin',(0.,0.,4.36808146));
#14949=CARTESIAN_POINT('',(-1.2,-1.46957615897682E-16,4.36808146));
#14950=CARTESIAN_POINT('Origin',(0.,0.,4.36808146));
#14951=CARTESIAN_POINT('Origin',(0.,0.,4.36808146));
#14952=CARTESIAN_POINT('Origin',(0.,0.,3.4));
#14953=CARTESIAN_POINT('',(-1.2,-1.46957615897682E-16,3.4));
#14954=CARTESIAN_POINT('',(-1.2,-1.46957615897682E-16,3.4));
#14955=CARTESIAN_POINT('Origin',(0.,0.,3.4));
#14956=CARTESIAN_POINT('Origin',(0.,0.,3.4));
#14957=CARTESIAN_POINT('Origin',(0.,0.,19.));
#14958=CARTESIAN_POINT('Origin',(0.29,-5.75,4.668081457105));
#14959=CARTESIAN_POINT('',(0.29,-5.88527749258469,4.57360923896654));
#14960=CARTESIAN_POINT('',(0.29,-5.61472250741531,4.57360923896654));
#14961=CARTESIAN_POINT('',(0.29,-6.1,4.57360923896654));
#14962=CARTESIAN_POINT('Origin',(0.29,-5.75,4.668081457105));
#14963=CARTESIAN_POINT('Origin',(0.29,-5.75,4.668081457105));
#14964=CARTESIAN_POINT('',(0.29,-5.88527749258469,4.76255367524346));
#14965=CARTESIAN_POINT('Ctrl Pts',(0.29,-5.88527749258469,4.76255367524346));
#14966=CARTESIAN_POINT('Ctrl Pts',(0.293078111442152,-5.89187616839667,
4.75310484112255));
#14967=CARTESIAN_POINT('Ctrl Pts',(0.295928845896546,-5.89761208817693,
4.7427508396533));
#14968=CARTESIAN_POINT('Ctrl Pts',(0.302593996394854,-5.91067507972101,
4.71157336496124));
#14969=CARTESIAN_POINT('Ctrl Pts',(0.305,-5.915,4.6892669703376));
#14970=CARTESIAN_POINT('Ctrl Pts',(0.305,-5.915,4.6468959438724));
#14971=CARTESIAN_POINT('Ctrl Pts',(0.302593996394854,-5.91067507972101,
4.62458954924876));
#14972=CARTESIAN_POINT('Ctrl Pts',(0.295928845896546,-5.89761208817693,
4.5934120745567));
#14973=CARTESIAN_POINT('Ctrl Pts',(0.293078111442152,-5.89187616839667,
4.58305807308745));
#14974=CARTESIAN_POINT('Ctrl Pts',(0.29,-5.88527749258469,4.57360923896654));
#14975=CARTESIAN_POINT('',(0.29,-5.75,4.833081457105));
#14976=CARTESIAN_POINT('Origin',(0.29,-5.75,4.668081457105));
#14977=CARTESIAN_POINT('',(0.8,-5.75,4.833081457105));
#14978=CARTESIAN_POINT('',(0.29,-5.75,4.833081457105));
#14979=CARTESIAN_POINT('Origin',(0.8,-5.75,4.668081457105));
#14980=CARTESIAN_POINT('',(0.29,-5.61472250741531,4.76255367524346));
#14981=CARTESIAN_POINT('Origin',(0.29,-5.75,4.668081457105));
#14982=CARTESIAN_POINT('Ctrl Pts',(0.29,-5.61472250741531,4.57360923896654));
#14983=CARTESIAN_POINT('Ctrl Pts',(0.293078111442152,-5.60812383160333,
4.58305807308745));
#14984=CARTESIAN_POINT('Ctrl Pts',(0.295928845896546,-5.60238791182307,
4.5934120745567));
#14985=CARTESIAN_POINT('Ctrl Pts',(0.302593996394854,-5.58932492027899,
4.62458954924876));
#14986=CARTESIAN_POINT('Ctrl Pts',(0.305,-5.585,4.6468959438724));
#14987=CARTESIAN_POINT('Ctrl Pts',(0.305,-5.585,4.6892669703376));
#14988=CARTESIAN_POINT('Ctrl Pts',(0.302593996394854,-5.58932492027899,
4.71157336496124));
#14989=CARTESIAN_POINT('Ctrl Pts',(0.295928845896546,-5.60238791182307,
4.7427508396533));
#14990=CARTESIAN_POINT('Ctrl Pts',(0.293078111442152,-5.60812383160333,
4.75310484112255));
#14991=CARTESIAN_POINT('Ctrl Pts',(0.29,-5.61472250741531,4.76255367524346));
#14992=CARTESIAN_POINT('Origin',(0.29,-5.75,4.668081457105));
#14993=CARTESIAN_POINT('',(0.29,-6.1,4.76255367524346));
#14994=CARTESIAN_POINT('Origin',(0.,-6.1,4.668081457105));
#14995=CARTESIAN_POINT('',(-0.305,-6.,4.668081457105));
#14996=CARTESIAN_POINT('Origin',(0.,-6.,4.668081457105));
#14997=CARTESIAN_POINT('',(-0.305,-5.51,4.668081457105));
#14998=CARTESIAN_POINT('',(-0.305,-6.1,4.668081457105));
#14999=CARTESIAN_POINT('Origin',(0.,-5.51,4.668081457105));
#15000=CARTESIAN_POINT('Origin',(-0.8,-6.,4.16808146));
#15001=CARTESIAN_POINT('',(-0.8,-6.,4.16808146));
#15002=CARTESIAN_POINT('',(0.8,-6.,4.16808146));
#15003=CARTESIAN_POINT('',(-0.8,-6.,4.16808146));
#15004=CARTESIAN_POINT('',(0.8,-6.,5.16808146));
#15005=CARTESIAN_POINT('',(0.8,-6.,4.16808146));
#15006=CARTESIAN_POINT('',(-0.8,-6.,5.16808146));
#15007=CARTESIAN_POINT('',(-0.8,-6.,5.16808146));
#15008=CARTESIAN_POINT('',(-0.8,-6.,4.16808146));
#15009=CARTESIAN_POINT('Origin',(-0.8,0.,4.16808146));
#15010=CARTESIAN_POINT('',(-0.8,-5.51,5.16808146));
#15011=CARTESIAN_POINT('',(-0.8,-5.51,4.16808146));
#15012=CARTESIAN_POINT('',(-0.8,-5.51,4.4180814585525));
#15013=CARTESIAN_POINT('',(-0.8,0.,4.16808146));
#15014=CARTESIAN_POINT('',(-0.8,0.,5.16808146));
#15015=CARTESIAN_POINT('Origin',(0.,-3.,5.16808146));
#15016=CARTESIAN_POINT('',(0.8,-5.51,5.16808146));
#15017=CARTESIAN_POINT('',(0.,-5.51,5.16808146));
#15018=CARTESIAN_POINT('',(0.8,-6.,5.16808146));
#15019=CARTESIAN_POINT('Origin',(0.,-3.,4.16808146));
#15020=CARTESIAN_POINT('',(0.8,-5.51,4.16808146));
#15021=CARTESIAN_POINT('',(0.,-5.51,4.16808146));
#15022=CARTESIAN_POINT('',(0.8,-6.,4.16808146));
#15023=CARTESIAN_POINT('Origin',(0.8,-6.,4.16808146));
#15024=CARTESIAN_POINT('',(0.8,-5.51,4.4180814585525));
#15025=CARTESIAN_POINT('Origin',(0.,-5.51,4.668081457105));
#15026=CARTESIAN_POINT('',(0.,0.,0.));
#15027=CARTESIAN_POINT('Origin',(0.,-6.,4.668081457105));
#15028=CARTESIAN_POINT('',(-0.5,-6.,4.668081457105));
#15029=CARTESIAN_POINT('Origin',(0.,-6.,4.668081457105));
#15030=CARTESIAN_POINT('',(-0.3,-6.,4.668081457105));
#15031=CARTESIAN_POINT('Origin',(0.,-6.,4.668081457105));
#15032=CARTESIAN_POINT('Origin',(0.,-6.2,4.668081457105));
#15033=CARTESIAN_POINT('',(-0.5,-6.2,4.668081457105));
#15034=CARTESIAN_POINT('',(-0.5,-6.2,4.668081457105));
#15035=CARTESIAN_POINT('Origin',(0.,-6.2,4.668081457105));
#15036=CARTESIAN_POINT('Origin',(0.,-6.2,4.668081457105));
#15037=CARTESIAN_POINT('Origin',(0.,-6.,4.668081457105));
#15038=CARTESIAN_POINT('',(-0.3,-3.9,4.668081457105));
#15039=CARTESIAN_POINT('Origin',(0.,-3.9,4.668081457105));
#15040=CARTESIAN_POINT('',(-0.3,-6.,4.668081457105));
#15041=CARTESIAN_POINT('Origin',(0.,-3.9,4.668081457105));
#15042=CARTESIAN_POINT('',(0.,0.,0.));
#15043=CARTESIAN_POINT('Origin',(0.,0.,3.));
#15044=CARTESIAN_POINT('',(-1.,-1.22464679914735E-16,3.4));
#15045=CARTESIAN_POINT('Origin',(0.,0.,3.4));
#15046=CARTESIAN_POINT('',(-1.,-1.22464679914735E-16,3.));
#15047=CARTESIAN_POINT('',(-1.,-1.22464679914735E-16,3.));
#15048=CARTESIAN_POINT('Origin',(0.,0.,3.));
#15049=CARTESIAN_POINT('Origin',(0.,0.,3.4));
#15050=CARTESIAN_POINT('Origin',(0.,0.,3.));
#15051=CARTESIAN_POINT('',(0.,0.,0.));
#15052=CARTESIAN_POINT('Origin',(0.0577350269189626,0.,-0.1));
#15053=CARTESIAN_POINT('',(0.0577350269189626,0.,-0.1));
#15054=CARTESIAN_POINT('',(0.115470053837925,0.,0.));
#15055=CARTESIAN_POINT('',(0.0934187836487032,0.,-0.0381939203391614));
#15056=CARTESIAN_POINT('',(0.0577350269189626,-0.2,-0.1));
#15057=CARTESIAN_POINT('',(0.0577350269189626,0.,-0.1));
#15058=CARTESIAN_POINT('',(0.115470053837925,-0.2,0.));
#15059=CARTESIAN_POINT('',(0.115470053837925,-0.2,0.));
#15060=CARTESIAN_POINT('',(0.115470053837925,0.,0.));
#15061=CARTESIAN_POINT('Origin',(-0.0577350269189626,0.,-0.1));
#15062=CARTESIAN_POINT('',(-0.0577350269189626,0.,-0.1));
#15063=CARTESIAN_POINT('',(0.0561324865405187,0.,-0.1));
#15064=CARTESIAN_POINT('',(-0.0577350269189626,-0.2,-0.1));
#15065=CARTESIAN_POINT('',(-0.0577350269189626,0.,-0.1));
#15066=CARTESIAN_POINT('',(0.0577350269189626,-0.2,-0.1));
#15067=CARTESIAN_POINT('Origin',(-0.115470053837925,0.,-1.38777878078145E-17));
#15068=CARTESIAN_POINT('',(-0.115470053837925,0.,-1.41410031829988E-17));
#15069=CARTESIAN_POINT('',(-0.0797862971081845,0.,-0.0618060796608387));
#15070=CARTESIAN_POINT('',(-0.115470053837925,-0.2,-1.38777878078145E-17));
#15071=CARTESIAN_POINT('',(-0.115470053837925,0.,-1.41410031829988E-17));
#15072=CARTESIAN_POINT('',(-0.0577350269189626,-0.2,-0.1));
#15073=CARTESIAN_POINT('Origin',(-0.0577350269189626,0.,0.1));
#15074=CARTESIAN_POINT('',(-0.0577350269189626,0.,0.1));
#15075=CARTESIAN_POINT('',(-0.0509187836487033,0.,0.111806079660839));
#15076=CARTESIAN_POINT('',(-0.0577350269189626,-0.2,0.1));
#15077=CARTESIAN_POINT('',(-0.0577350269189626,0.,0.1));
#15078=CARTESIAN_POINT('',(-0.115470053837925,-0.2,-1.41410031829988E-17));
#15079=CARTESIAN_POINT('Origin',(0.0577350269189626,0.,0.1));
#15080=CARTESIAN_POINT('',(0.0577350269189626,0.,0.1));
#15081=CARTESIAN_POINT('',(0.113867513459481,0.,0.1));
#15082=CARTESIAN_POINT('',(0.0577350269189626,-0.2,0.1));
#15083=CARTESIAN_POINT('',(0.0577350269189626,0.,0.1));
#15084=CARTESIAN_POINT('',(-0.0577350269189626,-0.2,0.1));
#15085=CARTESIAN_POINT('Origin',(0.115470053837925,0.,0.));
#15086=CARTESIAN_POINT('',(0.122286297108185,0.,-0.0118060796608386));
#15087=CARTESIAN_POINT('',(0.0577350269189626,-0.2,0.1));
#15088=CARTESIAN_POINT('Origin',(0.,-0.2,0.));
#15089=CARTESIAN_POINT('Origin',(0.17,0.,0.));
#15090=CARTESIAN_POINT('',(-0.17,-8.67361737988404E-18,-2.0818995585505E-17));
#15091=CARTESIAN_POINT('Origin',(0.,0.,0.));
#15092=CARTESIAN_POINT('Origin',(0.,-0.015,0.));
#15093=CARTESIAN_POINT('',(-0.1954,-0.0254,-2.39295984553393E-17));
#15094=CARTESIAN_POINT('Origin',(0.,-0.0254,0.));
#15095=CARTESIAN_POINT('',(-0.185,-0.015,-2.2655965784226E-17));
#15096=CARTESIAN_POINT('Origin',(0.,-0.2775,0.));
#15097=CARTESIAN_POINT('',(-0.1954,-0.5296,2.39295984553393E-17));
#15098=CARTESIAN_POINT('Origin',(0.,-0.5296,0.));
#15099=CARTESIAN_POINT('',(-0.1954,-0.2775,-2.39295984553393E-17));
#15100=CARTESIAN_POINT('Origin',(0.,-0.5625,0.));
#15101=CARTESIAN_POINT('',(-0.125,-0.6,-1.53080849893419E-17));
#15102=CARTESIAN_POINT('Origin',(0.,-0.6,0.));
#15103=CARTESIAN_POINT('',(-0.1625,-0.5625,-1.99005104861445E-17));
#15104=CARTESIAN_POINT('Origin',(0.,-0.6,0.));
#15105=CARTESIAN_POINT('',(0.,0.,0.));
#15106=CARTESIAN_POINT('',(0.,0.,0.));
#15107=CARTESIAN_POINT('',(0.,0.,0.));
#15108=CARTESIAN_POINT('',(0.9,-5.75,4.668081457105));
#15109=CARTESIAN_POINT('',(0.,0.,0.));
#15110=CARTESIAN_POINT('',(0.,0.,0.));
#15111=CARTESIAN_POINT('',(0.,0.,0.));
#15112=CARTESIAN_POINT('',(0.,0.,0.));
#15113=UNCERTAINTY_MEASURE_WITH_UNIT(LENGTH_MEASURE(0.001),#15213,
'DISTANCE_ACCURACY_VALUE',
'Maximum model space distance between geometric entities at asserted c
onnectivities');
#15114=UNCERTAINTY_MEASURE_WITH_UNIT(LENGTH_MEASURE(0.001),#15213,
'DISTANCE_ACCURACY_VALUE',
'Maximum model space distance between geometric entities at asserted c
onnectivities');
#15115=UNCERTAINTY_MEASURE_WITH_UNIT(LENGTH_MEASURE(0.001),#15213,
'DISTANCE_ACCURACY_VALUE',
'Maximum model space distance between geometric entities at asserted c
onnectivities');
#15116=UNCERTAINTY_MEASURE_WITH_UNIT(LENGTH_MEASURE(0.001),#15213,
'DISTANCE_ACCURACY_VALUE',
'Maximum model space distance between geometric entities at asserted c
onnectivities');
#15117=UNCERTAINTY_MEASURE_WITH_UNIT(LENGTH_MEASURE(0.001),#15213,
'DISTANCE_ACCURACY_VALUE',
'Maximum model space distance between geometric entities at asserted c
onnectivities');
#15118=UNCERTAINTY_MEASURE_WITH_UNIT(LENGTH_MEASURE(0.001),#15213,
'DISTANCE_ACCURACY_VALUE',
'Maximum model space distance between geometric entities at asserted c
onnectivities');
#15119=UNCERTAINTY_MEASURE_WITH_UNIT(LENGTH_MEASURE(0.001),#15213,
'DISTANCE_ACCURACY_VALUE',
'Maximum model space distance between geometric entities at asserted c
onnectivities');
#15120=UNCERTAINTY_MEASURE_WITH_UNIT(LENGTH_MEASURE(0.001),#15213,
'DISTANCE_ACCURACY_VALUE',
'Maximum model space distance between geometric entities at asserted c
onnectivities');
#15121=UNCERTAINTY_MEASURE_WITH_UNIT(LENGTH_MEASURE(0.001),#15213,
'DISTANCE_ACCURACY_VALUE',
'Maximum model space distance between geometric entities at asserted c
onnectivities');
#15122=UNCERTAINTY_MEASURE_WITH_UNIT(LENGTH_MEASURE(0.001),#15213,
'DISTANCE_ACCURACY_VALUE',
'Maximum model space distance between geometric entities at asserted c
onnectivities');
#15123=UNCERTAINTY_MEASURE_WITH_UNIT(LENGTH_MEASURE(0.001),#15213,
'DISTANCE_ACCURACY_VALUE',
'Maximum model space distance between geometric entities at asserted c
onnectivities');
#15124=UNCERTAINTY_MEASURE_WITH_UNIT(LENGTH_MEASURE(0.001),#15213,
'DISTANCE_ACCURACY_VALUE',
'Maximum model space distance between geometric entities at asserted c
onnectivities');
#15125=UNCERTAINTY_MEASURE_WITH_UNIT(LENGTH_MEASURE(0.001),#15213,
'DISTANCE_ACCURACY_VALUE',
'Maximum model space distance between geometric entities at asserted c
onnectivities');
#15126=UNCERTAINTY_MEASURE_WITH_UNIT(LENGTH_MEASURE(0.001),#15213,
'DISTANCE_ACCURACY_VALUE',
'Maximum model space distance between geometric entities at asserted c
onnectivities');
#15127=UNCERTAINTY_MEASURE_WITH_UNIT(LENGTH_MEASURE(0.001),#15213,
'DISTANCE_ACCURACY_VALUE',
'Maximum model space distance between geometric entities at asserted c
onnectivities');
#15128=UNCERTAINTY_MEASURE_WITH_UNIT(LENGTH_MEASURE(0.001),#15213,
'DISTANCE_ACCURACY_VALUE',
'Maximum model space distance between geometric entities at asserted c
onnectivities');
#15129=UNCERTAINTY_MEASURE_WITH_UNIT(LENGTH_MEASURE(0.001),#15213,
'DISTANCE_ACCURACY_VALUE',
'Maximum model space distance between geometric entities at asserted c
onnectivities');
#15130=UNCERTAINTY_MEASURE_WITH_UNIT(LENGTH_MEASURE(0.001),#15213,
'DISTANCE_ACCURACY_VALUE',
'Maximum model space distance between geometric entities at asserted c
onnectivities');
#15131=UNCERTAINTY_MEASURE_WITH_UNIT(LENGTH_MEASURE(0.001),#15213,
'DISTANCE_ACCURACY_VALUE',
'Maximum model space distance between geometric entities at asserted c
onnectivities');
#15132=UNCERTAINTY_MEASURE_WITH_UNIT(LENGTH_MEASURE(0.001),#15213,
'DISTANCE_ACCURACY_VALUE',
'Maximum model space distance between geometric entities at asserted c
onnectivities');
#15133=UNCERTAINTY_MEASURE_WITH_UNIT(LENGTH_MEASURE(0.001),#15213,
'DISTANCE_ACCURACY_VALUE',
'Maximum model space distance between geometric entities at asserted c
onnectivities');
#15134=UNCERTAINTY_MEASURE_WITH_UNIT(LENGTH_MEASURE(0.001),#15213,
'DISTANCE_ACCURACY_VALUE',
'Maximum model space distance between geometric entities at asserted c
onnectivities');
#15135=UNCERTAINTY_MEASURE_WITH_UNIT(LENGTH_MEASURE(0.001),#15213,
'DISTANCE_ACCURACY_VALUE',
'Maximum model space distance between geometric entities at asserted c
onnectivities');
#15136=UNCERTAINTY_MEASURE_WITH_UNIT(LENGTH_MEASURE(0.001),#15213,
'DISTANCE_ACCURACY_VALUE',
'Maximum model space distance between geometric entities at asserted c
onnectivities');
#15137=UNCERTAINTY_MEASURE_WITH_UNIT(LENGTH_MEASURE(0.001),#15213,
'DISTANCE_ACCURACY_VALUE',
'Maximum model space distance between geometric entities at asserted c
onnectivities');
#15138=UNCERTAINTY_MEASURE_WITH_UNIT(LENGTH_MEASURE(0.001),#15213,
'DISTANCE_ACCURACY_VALUE',
'Maximum model space distance between geometric entities at asserted c
onnectivities');
#15139=UNCERTAINTY_MEASURE_WITH_UNIT(LENGTH_MEASURE(0.001),#15213,
'DISTANCE_ACCURACY_VALUE',
'Maximum model space distance between geometric entities at asserted c
onnectivities');
#15140=UNCERTAINTY_MEASURE_WITH_UNIT(LENGTH_MEASURE(0.001),#15213,
'DISTANCE_ACCURACY_VALUE',
'Maximum model space distance between geometric entities at asserted c
onnectivities');
#15141=UNCERTAINTY_MEASURE_WITH_UNIT(LENGTH_MEASURE(0.001),#15213,
'DISTANCE_ACCURACY_VALUE',
'Maximum model space distance between geometric entities at asserted c
onnectivities');
#15142=UNCERTAINTY_MEASURE_WITH_UNIT(LENGTH_MEASURE(0.001),#15213,
'DISTANCE_ACCURACY_VALUE',
'Maximum model space distance between geometric entities at asserted c
onnectivities');
#15143=UNCERTAINTY_MEASURE_WITH_UNIT(LENGTH_MEASURE(0.001),#15213,
'DISTANCE_ACCURACY_VALUE',
'Maximum model space distance between geometric entities at asserted c
onnectivities');
#15144=UNCERTAINTY_MEASURE_WITH_UNIT(LENGTH_MEASURE(0.001),#15213,
'DISTANCE_ACCURACY_VALUE',
'Maximum model space distance between geometric entities at asserted c
onnectivities');
#15145=UNCERTAINTY_MEASURE_WITH_UNIT(LENGTH_MEASURE(0.001),#15213,
'DISTANCE_ACCURACY_VALUE',
'Maximum model space distance between geometric entities at asserted c
onnectivities');
#15146=UNCERTAINTY_MEASURE_WITH_UNIT(LENGTH_MEASURE(0.001),#15213,
'DISTANCE_ACCURACY_VALUE',
'Maximum model space distance between geometric entities at asserted c
onnectivities');
#15147=UNCERTAINTY_MEASURE_WITH_UNIT(LENGTH_MEASURE(0.001),#15213,
'DISTANCE_ACCURACY_VALUE',
'Maximum model space distance between geometric entities at asserted c
onnectivities');
#15148=UNCERTAINTY_MEASURE_WITH_UNIT(LENGTH_MEASURE(0.001),#15213,
'DISTANCE_ACCURACY_VALUE',
'Maximum model space distance between geometric entities at asserted c
onnectivities');
#15149=UNCERTAINTY_MEASURE_WITH_UNIT(LENGTH_MEASURE(0.001),#15213,
'DISTANCE_ACCURACY_VALUE',
'Maximum model space distance between geometric entities at asserted c
onnectivities');
#15150=UNCERTAINTY_MEASURE_WITH_UNIT(LENGTH_MEASURE(0.001),#15213,
'DISTANCE_ACCURACY_VALUE',
'Maximum model space distance between geometric entities at asserted c
onnectivities');
#15151=UNCERTAINTY_MEASURE_WITH_UNIT(LENGTH_MEASURE(0.001),#15213,
'DISTANCE_ACCURACY_VALUE',
'Maximum model space distance between geometric entities at asserted c
onnectivities');
#15152=UNCERTAINTY_MEASURE_WITH_UNIT(LENGTH_MEASURE(0.001),#15213,
'DISTANCE_ACCURACY_VALUE',
'Maximum model space distance between geometric entities at asserted c
onnectivities');
#15153=UNCERTAINTY_MEASURE_WITH_UNIT(LENGTH_MEASURE(0.001),#15213,
'DISTANCE_ACCURACY_VALUE',
'Maximum model space distance between geometric entities at asserted c
onnectivities');
#15154=UNCERTAINTY_MEASURE_WITH_UNIT(LENGTH_MEASURE(0.001),#15213,
'DISTANCE_ACCURACY_VALUE',
'Maximum model space distance between geometric entities at asserted c
onnectivities');
#15155=UNCERTAINTY_MEASURE_WITH_UNIT(LENGTH_MEASURE(0.001),#15213,
'DISTANCE_ACCURACY_VALUE',
'Maximum model space distance between geometric entities at asserted c
onnectivities');
#15156=UNCERTAINTY_MEASURE_WITH_UNIT(LENGTH_MEASURE(0.001),#15213,
'DISTANCE_ACCURACY_VALUE',
'Maximum model space distance between geometric entities at asserted c
onnectivities');
#15157=UNCERTAINTY_MEASURE_WITH_UNIT(LENGTH_MEASURE(0.001),#15213,
'DISTANCE_ACCURACY_VALUE',
'Maximum model space distance between geometric entities at asserted c
onnectivities');
#15158=UNCERTAINTY_MEASURE_WITH_UNIT(LENGTH_MEASURE(0.001),#15213,
'DISTANCE_ACCURACY_VALUE',
'Maximum model space distance between geometric entities at asserted c
onnectivities');
#15159=UNCERTAINTY_MEASURE_WITH_UNIT(LENGTH_MEASURE(0.001),#15213,
'DISTANCE_ACCURACY_VALUE',
'Maximum model space distance between geometric entities at asserted c
onnectivities');
#15160=UNCERTAINTY_MEASURE_WITH_UNIT(LENGTH_MEASURE(0.001),#15213,
'DISTANCE_ACCURACY_VALUE',
'Maximum model space distance between geometric entities at asserted c
onnectivities');
#15161=UNCERTAINTY_MEASURE_WITH_UNIT(LENGTH_MEASURE(0.001),#15213,
'DISTANCE_ACCURACY_VALUE',
'Maximum model space distance between geometric entities at asserted c
onnectivities');
#15162=UNCERTAINTY_MEASURE_WITH_UNIT(LENGTH_MEASURE(0.001),#15213,
'DISTANCE_ACCURACY_VALUE',
'Maximum model space distance between geometric entities at asserted c
onnectivities');
#15163=(
GEOMETRIC_REPRESENTATION_CONTEXT(3)
GLOBAL_UNCERTAINTY_ASSIGNED_CONTEXT((#15113))
GLOBAL_UNIT_ASSIGNED_CONTEXT((#15213,#15215,#15216))
REPRESENTATION_CONTEXT('','3D')
);
#15164=(
GEOMETRIC_REPRESENTATION_CONTEXT(3)
GLOBAL_UNCERTAINTY_ASSIGNED_CONTEXT((#15114))
GLOBAL_UNIT_ASSIGNED_CONTEXT((#15213,#15215,#15216))
REPRESENTATION_CONTEXT('','3D')
);
#15165=(
GEOMETRIC_REPRESENTATION_CONTEXT(3)
GLOBAL_UNCERTAINTY_ASSIGNED_CONTEXT((#15115))
GLOBAL_UNIT_ASSIGNED_CONTEXT((#15213,#15215,#15216))
REPRESENTATION_CONTEXT('','3D')
);
#15166=(
GEOMETRIC_REPRESENTATION_CONTEXT(3)
GLOBAL_UNCERTAINTY_ASSIGNED_CONTEXT((#15116))
GLOBAL_UNIT_ASSIGNED_CONTEXT((#15213,#15215,#15216))
REPRESENTATION_CONTEXT('','3D')
);
#15167=(
GEOMETRIC_REPRESENTATION_CONTEXT(3)
GLOBAL_UNCERTAINTY_ASSIGNED_CONTEXT((#15117))
GLOBAL_UNIT_ASSIGNED_CONTEXT((#15213,#15215,#15216))
REPRESENTATION_CONTEXT('','3D')
);
#15168=(
GEOMETRIC_REPRESENTATION_CONTEXT(3)
GLOBAL_UNCERTAINTY_ASSIGNED_CONTEXT((#15118))
GLOBAL_UNIT_ASSIGNED_CONTEXT((#15213,#15215,#15216))
REPRESENTATION_CONTEXT('','3D')
);
#15169=(
GEOMETRIC_REPRESENTATION_CONTEXT(3)
GLOBAL_UNCERTAINTY_ASSIGNED_CONTEXT((#15119))
GLOBAL_UNIT_ASSIGNED_CONTEXT((#15213,#15215,#15216))
REPRESENTATION_CONTEXT('','3D')
);
#15170=(
GEOMETRIC_REPRESENTATION_CONTEXT(3)
GLOBAL_UNCERTAINTY_ASSIGNED_CONTEXT((#15120))
GLOBAL_UNIT_ASSIGNED_CONTEXT((#15213,#15215,#15216))
REPRESENTATION_CONTEXT('','3D')
);
#15171=(
GEOMETRIC_REPRESENTATION_CONTEXT(3)
GLOBAL_UNCERTAINTY_ASSIGNED_CONTEXT((#15121))
GLOBAL_UNIT_ASSIGNED_CONTEXT((#15213,#15215,#15216))
REPRESENTATION_CONTEXT('','3D')
);
#15172=(
GEOMETRIC_REPRESENTATION_CONTEXT(3)
GLOBAL_UNCERTAINTY_ASSIGNED_CONTEXT((#15122))
GLOBAL_UNIT_ASSIGNED_CONTEXT((#15213,#15215,#15216))
REPRESENTATION_CONTEXT('','3D')
);
#15173=(
GEOMETRIC_REPRESENTATION_CONTEXT(3)
GLOBAL_UNCERTAINTY_ASSIGNED_CONTEXT((#15123))
GLOBAL_UNIT_ASSIGNED_CONTEXT((#15213,#15215,#15216))
REPRESENTATION_CONTEXT('','3D')
);
#15174=(
GEOMETRIC_REPRESENTATION_CONTEXT(3)
GLOBAL_UNCERTAINTY_ASSIGNED_CONTEXT((#15124))
GLOBAL_UNIT_ASSIGNED_CONTEXT((#15213,#15215,#15216))
REPRESENTATION_CONTEXT('','3D')
);
#15175=(
GEOMETRIC_REPRESENTATION_CONTEXT(3)
GLOBAL_UNCERTAINTY_ASSIGNED_CONTEXT((#15125))
GLOBAL_UNIT_ASSIGNED_CONTEXT((#15213,#15215,#15216))
REPRESENTATION_CONTEXT('','3D')
);
#15176=(
GEOMETRIC_REPRESENTATION_CONTEXT(3)
GLOBAL_UNCERTAINTY_ASSIGNED_CONTEXT((#15126))
GLOBAL_UNIT_ASSIGNED_CONTEXT((#15213,#15215,#15216))
REPRESENTATION_CONTEXT('','3D')
);
#15177=(
GEOMETRIC_REPRESENTATION_CONTEXT(3)
GLOBAL_UNCERTAINTY_ASSIGNED_CONTEXT((#15127))
GLOBAL_UNIT_ASSIGNED_CONTEXT((#15213,#15215,#15216))
REPRESENTATION_CONTEXT('','3D')
);
#15178=(
GEOMETRIC_REPRESENTATION_CONTEXT(3)
GLOBAL_UNCERTAINTY_ASSIGNED_CONTEXT((#15128))
GLOBAL_UNIT_ASSIGNED_CONTEXT((#15213,#15215,#15216))
REPRESENTATION_CONTEXT('','3D')
);
#15179=(
GEOMETRIC_REPRESENTATION_CONTEXT(3)
GLOBAL_UNCERTAINTY_ASSIGNED_CONTEXT((#15129))
GLOBAL_UNIT_ASSIGNED_CONTEXT((#15213,#15215,#15216))
REPRESENTATION_CONTEXT('','3D')
);
#15180=(
GEOMETRIC_REPRESENTATION_CONTEXT(3)
GLOBAL_UNCERTAINTY_ASSIGNED_CONTEXT((#15130))
GLOBAL_UNIT_ASSIGNED_CONTEXT((#15213,#15215,#15216))
REPRESENTATION_CONTEXT('','3D')
);
#15181=(
GEOMETRIC_REPRESENTATION_CONTEXT(3)
GLOBAL_UNCERTAINTY_ASSIGNED_CONTEXT((#15131))
GLOBAL_UNIT_ASSIGNED_CONTEXT((#15213,#15215,#15216))
REPRESENTATION_CONTEXT('','3D')
);
#15182=(
GEOMETRIC_REPRESENTATION_CONTEXT(3)
GLOBAL_UNCERTAINTY_ASSIGNED_CONTEXT((#15132))
GLOBAL_UNIT_ASSIGNED_CONTEXT((#15213,#15215,#15216))
REPRESENTATION_CONTEXT('','3D')
);
#15183=(
GEOMETRIC_REPRESENTATION_CONTEXT(3)
GLOBAL_UNCERTAINTY_ASSIGNED_CONTEXT((#15133))
GLOBAL_UNIT_ASSIGNED_CONTEXT((#15213,#15215,#15216))
REPRESENTATION_CONTEXT('','3D')
);
#15184=(
GEOMETRIC_REPRESENTATION_CONTEXT(3)
GLOBAL_UNCERTAINTY_ASSIGNED_CONTEXT((#15134))
GLOBAL_UNIT_ASSIGNED_CONTEXT((#15213,#15215,#15216))
REPRESENTATION_CONTEXT('','3D')
);
#15185=(
GEOMETRIC_REPRESENTATION_CONTEXT(3)
GLOBAL_UNCERTAINTY_ASSIGNED_CONTEXT((#15135))
GLOBAL_UNIT_ASSIGNED_CONTEXT((#15213,#15215,#15216))
REPRESENTATION_CONTEXT('','3D')
);
#15186=(
GEOMETRIC_REPRESENTATION_CONTEXT(3)
GLOBAL_UNCERTAINTY_ASSIGNED_CONTEXT((#15136))
GLOBAL_UNIT_ASSIGNED_CONTEXT((#15213,#15215,#15216))
REPRESENTATION_CONTEXT('','3D')
);
#15187=(
GEOMETRIC_REPRESENTATION_CONTEXT(3)
GLOBAL_UNCERTAINTY_ASSIGNED_CONTEXT((#15137))
GLOBAL_UNIT_ASSIGNED_CONTEXT((#15213,#15215,#15216))
REPRESENTATION_CONTEXT('','3D')
);
#15188=(
GEOMETRIC_REPRESENTATION_CONTEXT(3)
GLOBAL_UNCERTAINTY_ASSIGNED_CONTEXT((#15138))
GLOBAL_UNIT_ASSIGNED_CONTEXT((#15213,#15215,#15216))
REPRESENTATION_CONTEXT('','3D')
);
#15189=(
GEOMETRIC_REPRESENTATION_CONTEXT(3)
GLOBAL_UNCERTAINTY_ASSIGNED_CONTEXT((#15139))
GLOBAL_UNIT_ASSIGNED_CONTEXT((#15213,#15215,#15216))
REPRESENTATION_CONTEXT('','3D')
);
#15190=(
GEOMETRIC_REPRESENTATION_CONTEXT(3)
GLOBAL_UNCERTAINTY_ASSIGNED_CONTEXT((#15140))
GLOBAL_UNIT_ASSIGNED_CONTEXT((#15213,#15215,#15216))
REPRESENTATION_CONTEXT('','3D')
);
#15191=(
GEOMETRIC_REPRESENTATION_CONTEXT(3)
GLOBAL_UNCERTAINTY_ASSIGNED_CONTEXT((#15141))
GLOBAL_UNIT_ASSIGNED_CONTEXT((#15213,#15215,#15216))
REPRESENTATION_CONTEXT('','3D')
);
#15192=(
GEOMETRIC_REPRESENTATION_CONTEXT(3)
GLOBAL_UNCERTAINTY_ASSIGNED_CONTEXT((#15142))
GLOBAL_UNIT_ASSIGNED_CONTEXT((#15213,#15215,#15216))
REPRESENTATION_CONTEXT('','3D')
);
#15193=(
GEOMETRIC_REPRESENTATION_CONTEXT(3)
GLOBAL_UNCERTAINTY_ASSIGNED_CONTEXT((#15143))
GLOBAL_UNIT_ASSIGNED_CONTEXT((#15213,#15215,#15216))
REPRESENTATION_CONTEXT('','3D')
);
#15194=(
GEOMETRIC_REPRESENTATION_CONTEXT(3)
GLOBAL_UNCERTAINTY_ASSIGNED_CONTEXT((#15144))
GLOBAL_UNIT_ASSIGNED_CONTEXT((#15213,#15215,#15216))
REPRESENTATION_CONTEXT('','3D')
);
#15195=(
GEOMETRIC_REPRESENTATION_CONTEXT(3)
GLOBAL_UNCERTAINTY_ASSIGNED_CONTEXT((#15145))
GLOBAL_UNIT_ASSIGNED_CONTEXT((#15213,#15215,#15216))
REPRESENTATION_CONTEXT('','3D')
);
#15196=(
GEOMETRIC_REPRESENTATION_CONTEXT(3)
GLOBAL_UNCERTAINTY_ASSIGNED_CONTEXT((#15146))
GLOBAL_UNIT_ASSIGNED_CONTEXT((#15213,#15215,#15216))
REPRESENTATION_CONTEXT('','3D')
);
#15197=(
GEOMETRIC_REPRESENTATION_CONTEXT(3)
GLOBAL_UNCERTAINTY_ASSIGNED_CONTEXT((#15147))
GLOBAL_UNIT_ASSIGNED_CONTEXT((#15213,#15215,#15216))
REPRESENTATION_CONTEXT('','3D')
);
#15198=(
GEOMETRIC_REPRESENTATION_CONTEXT(3)
GLOBAL_UNCERTAINTY_ASSIGNED_CONTEXT((#15148))
GLOBAL_UNIT_ASSIGNED_CONTEXT((#15213,#15215,#15216))
REPRESENTATION_CONTEXT('','3D')
);
#15199=(
GEOMETRIC_REPRESENTATION_CONTEXT(3)
GLOBAL_UNCERTAINTY_ASSIGNED_CONTEXT((#15149))
GLOBAL_UNIT_ASSIGNED_CONTEXT((#15213,#15215,#15216))
REPRESENTATION_CONTEXT('','3D')
);
#15200=(
GEOMETRIC_REPRESENTATION_CONTEXT(3)
GLOBAL_UNCERTAINTY_ASSIGNED_CONTEXT((#15150))
GLOBAL_UNIT_ASSIGNED_CONTEXT((#15213,#15215,#15216))
REPRESENTATION_CONTEXT('','3D')
);
#15201=(
GEOMETRIC_REPRESENTATION_CONTEXT(3)
GLOBAL_UNCERTAINTY_ASSIGNED_CONTEXT((#15151))
GLOBAL_UNIT_ASSIGNED_CONTEXT((#15213,#15215,#15216))
REPRESENTATION_CONTEXT('','3D')
);
#15202=(
GEOMETRIC_REPRESENTATION_CONTEXT(3)
GLOBAL_UNCERTAINTY_ASSIGNED_CONTEXT((#15152))
GLOBAL_UNIT_ASSIGNED_CONTEXT((#15213,#15215,#15216))
REPRESENTATION_CONTEXT('','3D')
);
#15203=(
GEOMETRIC_REPRESENTATION_CONTEXT(3)
GLOBAL_UNCERTAINTY_ASSIGNED_CONTEXT((#15153))
GLOBAL_UNIT_ASSIGNED_CONTEXT((#15213,#15215,#15216))
REPRESENTATION_CONTEXT('','3D')
);
#15204=(
GEOMETRIC_REPRESENTATION_CONTEXT(3)
GLOBAL_UNCERTAINTY_ASSIGNED_CONTEXT((#15154))
GLOBAL_UNIT_ASSIGNED_CONTEXT((#15213,#15215,#15216))
REPRESENTATION_CONTEXT('','3D')
);
#15205=(
GEOMETRIC_REPRESENTATION_CONTEXT(3)
GLOBAL_UNCERTAINTY_ASSIGNED_CONTEXT((#15155))
GLOBAL_UNIT_ASSIGNED_CONTEXT((#15213,#15215,#15216))
REPRESENTATION_CONTEXT('','3D')
);
#15206=(
GEOMETRIC_REPRESENTATION_CONTEXT(3)
GLOBAL_UNCERTAINTY_ASSIGNED_CONTEXT((#15156))
GLOBAL_UNIT_ASSIGNED_CONTEXT((#15213,#15215,#15216))
REPRESENTATION_CONTEXT('','3D')
);
#15207=(
GEOMETRIC_REPRESENTATION_CONTEXT(3)
GLOBAL_UNCERTAINTY_ASSIGNED_CONTEXT((#15157))
GLOBAL_UNIT_ASSIGNED_CONTEXT((#15213,#15215,#15216))
REPRESENTATION_CONTEXT('','3D')
);
#15208=(
GEOMETRIC_REPRESENTATION_CONTEXT(3)
GLOBAL_UNCERTAINTY_ASSIGNED_CONTEXT((#15158))
GLOBAL_UNIT_ASSIGNED_CONTEXT((#15213,#15215,#15216))
REPRESENTATION_CONTEXT('','3D')
);
#15209=(
GEOMETRIC_REPRESENTATION_CONTEXT(3)
GLOBAL_UNCERTAINTY_ASSIGNED_CONTEXT((#15159))
GLOBAL_UNIT_ASSIGNED_CONTEXT((#15213,#15215,#15216))
REPRESENTATION_CONTEXT('','3D')
);
#15210=(
GEOMETRIC_REPRESENTATION_CONTEXT(3)
GLOBAL_UNCERTAINTY_ASSIGNED_CONTEXT((#15160))
GLOBAL_UNIT_ASSIGNED_CONTEXT((#15213,#15215,#15216))
REPRESENTATION_CONTEXT('','3D')
);
#15211=(
GEOMETRIC_REPRESENTATION_CONTEXT(3)
GLOBAL_UNCERTAINTY_ASSIGNED_CONTEXT((#15161))
GLOBAL_UNIT_ASSIGNED_CONTEXT((#15213,#15215,#15216))
REPRESENTATION_CONTEXT('','3D')
);
#15212=(
GEOMETRIC_REPRESENTATION_CONTEXT(3)
GLOBAL_UNCERTAINTY_ASSIGNED_CONTEXT((#15162))
GLOBAL_UNIT_ASSIGNED_CONTEXT((#15213,#15215,#15216))
REPRESENTATION_CONTEXT('','3D')
);
#15213=(
LENGTH_UNIT()
NAMED_UNIT(*)
SI_UNIT(.CENTI.,.METRE.)
);
#15214=(
LENGTH_UNIT()
NAMED_UNIT(*)
SI_UNIT($,.METRE.)
);
#15215=(
NAMED_UNIT(*)
PLANE_ANGLE_UNIT()
SI_UNIT($,.RADIAN.)
);
#15216=(
NAMED_UNIT(*)
SI_UNIT($,.STERADIAN.)
SOLID_ANGLE_UNIT()
);
#15217=SHAPE_DEFINITION_REPRESENTATION(#15266,#15401);
#15218=SHAPE_DEFINITION_REPRESENTATION(#15267,#15402);
#15219=SHAPE_DEFINITION_REPRESENTATION(#15268,#15403);
#15220=SHAPE_DEFINITION_REPRESENTATION(#15269,#15404);
#15221=SHAPE_DEFINITION_REPRESENTATION(#15270,#15405);
#15222=SHAPE_DEFINITION_REPRESENTATION(#15271,#15406);
#15223=SHAPE_DEFINITION_REPRESENTATION(#15272,#15407);
#15224=SHAPE_DEFINITION_REPRESENTATION(#15273,#15408);
#15225=SHAPE_DEFINITION_REPRESENTATION(#15274,#15409);
#15226=SHAPE_DEFINITION_REPRESENTATION(#15275,#15410);
#15227=SHAPE_DEFINITION_REPRESENTATION(#15276,#15411);
#15228=SHAPE_DEFINITION_REPRESENTATION(#15277,#15412);
#15229=SHAPE_DEFINITION_REPRESENTATION(#15278,#15413);
#15230=SHAPE_DEFINITION_REPRESENTATION(#15279,#15414);
#15231=SHAPE_DEFINITION_REPRESENTATION(#15280,#15415);
#15232=SHAPE_DEFINITION_REPRESENTATION(#15281,#15416);
#15233=SHAPE_DEFINITION_REPRESENTATION(#15282,#15417);
#15234=SHAPE_DEFINITION_REPRESENTATION(#15283,#15418);
#15235=SHAPE_DEFINITION_REPRESENTATION(#15284,#15419);
#15236=SHAPE_DEFINITION_REPRESENTATION(#15285,#15420);
#15237=SHAPE_DEFINITION_REPRESENTATION(#15286,#15421);
#15238=SHAPE_DEFINITION_REPRESENTATION(#15287,#15422);
#15239=SHAPE_DEFINITION_REPRESENTATION(#15288,#15423);
#15240=SHAPE_DEFINITION_REPRESENTATION(#15289,#15424);
#15241=SHAPE_DEFINITION_REPRESENTATION(#15295,#15425);
#15242=SHAPE_DEFINITION_REPRESENTATION(#15296,#15426);
#15243=SHAPE_DEFINITION_REPRESENTATION(#15297,#15427);
#15244=SHAPE_DEFINITION_REPRESENTATION(#15300,#15428);
#15245=SHAPE_DEFINITION_REPRESENTATION(#15301,#15429);
#15246=SHAPE_DEFINITION_REPRESENTATION(#15302,#15430);
#15247=SHAPE_DEFINITION_REPRESENTATION(#15303,#15431);
#15248=SHAPE_DEFINITION_REPRESENTATION(#15304,#15432);
#15249=SHAPE_DEFINITION_REPRESENTATION(#15305,#15433);
#15250=SHAPE_DEFINITION_REPRESENTATION(#15306,#15434);
#15251=SHAPE_DEFINITION_REPRESENTATION(#15307,#15435);
#15252=SHAPE_DEFINITION_REPRESENTATION(#15308,#15436);
#15253=SHAPE_DEFINITION_REPRESENTATION(#15309,#15437);
#15254=SHAPE_DEFINITION_REPRESENTATION(#15310,#15438);
#15255=SHAPE_DEFINITION_REPRESENTATION(#15311,#15439);
#15256=SHAPE_DEFINITION_REPRESENTATION(#15312,#15440);
#15257=SHAPE_DEFINITION_REPRESENTATION(#15381,#15441);
#15258=SHAPE_DEFINITION_REPRESENTATION(#15382,#15442);
#15259=SHAPE_DEFINITION_REPRESENTATION(#15383,#15443);
#15260=SHAPE_DEFINITION_REPRESENTATION(#15384,#15444);
#15261=SHAPE_DEFINITION_REPRESENTATION(#15388,#15445);
#15262=SHAPE_DEFINITION_REPRESENTATION(#15389,#15446);
#15263=SHAPE_DEFINITION_REPRESENTATION(#15390,#15447);
#15264=SHAPE_DEFINITION_REPRESENTATION(#15391,#15448);
#15265=SHAPE_DEFINITION_REPRESENTATION(#15392,#15449);
#15266=PRODUCT_DEFINITION_SHAPE('',$,#15451);
#15267=PRODUCT_DEFINITION_SHAPE('',$,#15452);
#15268=PRODUCT_DEFINITION_SHAPE('',$,#15453);
#15269=PRODUCT_DEFINITION_SHAPE('',$,#15454);
#15270=PRODUCT_DEFINITION_SHAPE('',$,#15455);
#15271=PRODUCT_DEFINITION_SHAPE('',$,#15456);
#15272=PRODUCT_DEFINITION_SHAPE('',$,#15457);
#15273=PRODUCT_DEFINITION_SHAPE('',$,#15458);
#15274=PRODUCT_DEFINITION_SHAPE('',$,#15459);
#15275=PRODUCT_DEFINITION_SHAPE('',$,#15460);
#15276=PRODUCT_DEFINITION_SHAPE('',$,#15461);
#15277=PRODUCT_DEFINITION_SHAPE('',$,#15462);
#15278=PRODUCT_DEFINITION_SHAPE('',$,#15463);
#15279=PRODUCT_DEFINITION_SHAPE('',$,#15464);
#15280=PRODUCT_DEFINITION_SHAPE('',$,#15465);
#15281=PRODUCT_DEFINITION_SHAPE('',$,#15466);
#15282=PRODUCT_DEFINITION_SHAPE('',$,#15467);
#15283=PRODUCT_DEFINITION_SHAPE('',$,#15468);
#15284=PRODUCT_DEFINITION_SHAPE('',$,#15469);
#15285=PRODUCT_DEFINITION_SHAPE('',$,#15470);
#15286=PRODUCT_DEFINITION_SHAPE('',$,#15471);
#15287=PRODUCT_DEFINITION_SHAPE('',$,#15472);
#15288=PRODUCT_DEFINITION_SHAPE('',$,#15473);
#15289=PRODUCT_DEFINITION_SHAPE('',$,#15474);
#15290=PRODUCT_DEFINITION_SHAPE($,$,#269);
#15291=PRODUCT_DEFINITION_SHAPE($,$,#270);
#15292=PRODUCT_DEFINITION_SHAPE($,$,#271);
#15293=PRODUCT_DEFINITION_SHAPE($,$,#272);
#15294=PRODUCT_DEFINITION_SHAPE($,$,#273);
#15295=PRODUCT_DEFINITION_SHAPE('',$,#15475);
#15296=PRODUCT_DEFINITION_SHAPE('',$,#15476);
#15297=PRODUCT_DEFINITION_SHAPE('',$,#15477);
#15298=PRODUCT_DEFINITION_SHAPE($,$,#274);
#15299=PRODUCT_DEFINITION_SHAPE($,$,#275);
#15300=PRODUCT_DEFINITION_SHAPE('',$,#15478);
#15301=PRODUCT_DEFINITION_SHAPE('',$,#15479);
#15302=PRODUCT_DEFINITION_SHAPE('',$,#15480);
#15303=PRODUCT_DEFINITION_SHAPE('',$,#15481);
#15304=PRODUCT_DEFINITION_SHAPE('',$,#15482);
#15305=PRODUCT_DEFINITION_SHAPE('',$,#15483);
#15306=PRODUCT_DEFINITION_SHAPE('',$,#15484);
#15307=PRODUCT_DEFINITION_SHAPE('',$,#15485);
#15308=PRODUCT_DEFINITION_SHAPE('',$,#15486);
#15309=PRODUCT_DEFINITION_SHAPE('',$,#15487);
#15310=PRODUCT_DEFINITION_SHAPE('',$,#15488);
#15311=PRODUCT_DEFINITION_SHAPE('',$,#15489);
#15312=PRODUCT_DEFINITION_SHAPE('',$,#15490);
#15313=PRODUCT_DEFINITION_SHAPE($,$,#276);
#15314=PRODUCT_DEFINITION_SHAPE($,$,#277);
#15315=PRODUCT_DEFINITION_SHAPE($,$,#278);
#15316=PRODUCT_DEFINITION_SHAPE($,$,#279);
#15317=PRODUCT_DEFINITION_SHAPE($,$,#280);
#15318=PRODUCT_DEFINITION_SHAPE($,$,#281);
#15319=PRODUCT_DEFINITION_SHAPE($,$,#282);
#15320=PRODUCT_DEFINITION_SHAPE($,$,#283);
#15321=PRODUCT_DEFINITION_SHAPE($,$,#284);
#15322=PRODUCT_DEFINITION_SHAPE($,$,#285);
#15323=PRODUCT_DEFINITION_SHAPE($,$,#286);
#15324=PRODUCT_DEFINITION_SHAPE($,$,#287);
#15325=PRODUCT_DEFINITION_SHAPE($,$,#288);
#15326=PRODUCT_DEFINITION_SHAPE($,$,#289);
#15327=PRODUCT_DEFINITION_SHAPE($,$,#290);
#15328=PRODUCT_DEFINITION_SHAPE($,$,#291);
#15329=PRODUCT_DEFINITION_SHAPE($,$,#292);
#15330=PRODUCT_DEFINITION_SHAPE($,$,#293);
#15331=PRODUCT_DEFINITION_SHAPE($,$,#294);
#15332=PRODUCT_DEFINITION_SHAPE($,$,#295);
#15333=PRODUCT_DEFINITION_SHAPE($,$,#296);
#15334=PRODUCT_DEFINITION_SHAPE($,$,#297);
#15335=PRODUCT_DEFINITION_SHAPE($,$,#298);
#15336=PRODUCT_DEFINITION_SHAPE($,$,#299);
#15337=PRODUCT_DEFINITION_SHAPE($,$,#300);
#15338=PRODUCT_DEFINITION_SHAPE($,$,#301);
#15339=PRODUCT_DEFINITION_SHAPE($,$,#302);
#15340=PRODUCT_DEFINITION_SHAPE($,$,#303);
#15341=PRODUCT_DEFINITION_SHAPE($,$,#304);
#15342=PRODUCT_DEFINITION_SHAPE($,$,#305);
#15343=PRODUCT_DEFINITION_SHAPE($,$,#306);
#15344=PRODUCT_DEFINITION_SHAPE($,$,#307);
#15345=PRODUCT_DEFINITION_SHAPE($,$,#308);
#15346=PRODUCT_DEFINITION_SHAPE($,$,#309);
#15347=PRODUCT_DEFINITION_SHAPE($,$,#310);
#15348=PRODUCT_DEFINITION_SHAPE($,$,#311);
#15349=PRODUCT_DEFINITION_SHAPE($,$,#312);
#15350=PRODUCT_DEFINITION_SHAPE($,$,#313);
#15351=PRODUCT_DEFINITION_SHAPE($,$,#314);
#15352=PRODUCT_DEFINITION_SHAPE($,$,#315);
#15353=PRODUCT_DEFINITION_SHAPE($,$,#316);
#15354=PRODUCT_DEFINITION_SHAPE($,$,#317);
#15355=PRODUCT_DEFINITION_SHAPE($,$,#318);
#15356=PRODUCT_DEFINITION_SHAPE($,$,#319);
#15357=PRODUCT_DEFINITION_SHAPE($,$,#320);
#15358=PRODUCT_DEFINITION_SHAPE($,$,#321);
#15359=PRODUCT_DEFINITION_SHAPE($,$,#322);
#15360=PRODUCT_DEFINITION_SHAPE($,$,#323);
#15361=PRODUCT_DEFINITION_SHAPE($,$,#324);
#15362=PRODUCT_DEFINITION_SHAPE($,$,#325);
#15363=PRODUCT_DEFINITION_SHAPE($,$,#326);
#15364=PRODUCT_DEFINITION_SHAPE($,$,#327);
#15365=PRODUCT_DEFINITION_SHAPE($,$,#328);
#15366=PRODUCT_DEFINITION_SHAPE($,$,#329);
#15367=PRODUCT_DEFINITION_SHAPE($,$,#330);
#15368=PRODUCT_DEFINITION_SHAPE($,$,#331);
#15369=PRODUCT_DEFINITION_SHAPE($,$,#332);
#15370=PRODUCT_DEFINITION_SHAPE($,$,#333);
#15371=PRODUCT_DEFINITION_SHAPE($,$,#334);
#15372=PRODUCT_DEFINITION_SHAPE($,$,#335);
#15373=PRODUCT_DEFINITION_SHAPE($,$,#336);
#15374=PRODUCT_DEFINITION_SHAPE($,$,#337);
#15375=PRODUCT_DEFINITION_SHAPE($,$,#338);
#15376=PRODUCT_DEFINITION_SHAPE($,$,#339);
#15377=PRODUCT_DEFINITION_SHAPE($,$,#340);
#15378=PRODUCT_DEFINITION_SHAPE($,$,#341);
#15379=PRODUCT_DEFINITION_SHAPE($,$,#342);
#15380=PRODUCT_DEFINITION_SHAPE($,$,#343);
#15381=PRODUCT_DEFINITION_SHAPE('',$,#15491);
#15382=PRODUCT_DEFINITION_SHAPE('',$,#15492);
#15383=PRODUCT_DEFINITION_SHAPE('',$,#15493);
#15384=PRODUCT_DEFINITION_SHAPE('',$,#15494);
#15385=PRODUCT_DEFINITION_SHAPE($,$,#344);
#15386=PRODUCT_DEFINITION_SHAPE($,$,#345);
#15387=PRODUCT_DEFINITION_SHAPE($,$,#346);
#15388=PRODUCT_DEFINITION_SHAPE('',$,#15495);
#15389=PRODUCT_DEFINITION_SHAPE('',$,#15496);
#15390=PRODUCT_DEFINITION_SHAPE('',$,#15497);
#15391=PRODUCT_DEFINITION_SHAPE('',$,#15498);
#15392=PRODUCT_DEFINITION_SHAPE('',$,#15499);
#15393=PRODUCT_DEFINITION_SHAPE($,$,#347);
#15394=PRODUCT_DEFINITION_SHAPE($,$,#348);
#15395=PRODUCT_DEFINITION_SHAPE($,$,#349);
#15396=PRODUCT_DEFINITION_SHAPE($,$,#350);
#15397=PRODUCT_DEFINITION_SHAPE($,$,#351);
#15398=PRODUCT_DEFINITION_SHAPE($,$,#352);
#15399=PRODUCT_DEFINITION_SHAPE($,$,#353);
#15400=PRODUCT_DEFINITION_SHAPE($,$,#354);
#15401=SHAPE_REPRESENTATION('',(#8763,#9750,#9751,#9752,#9753),#15163);
#15402=SHAPE_REPRESENTATION('',(#8764,#9565,#9566,#9567,#9568,#9569,#9570,
#9571,#9572,#9573,#9574,#9575,#9576,#9577,#9578,#9579,#9580,#9581,#9582,
#9583,#9584,#9585,#9586,#9587,#9588,#9589,#9590,#9591,#9592,#9593,#9594,
#9595,#9596,#9597,#9598,#9599,#9600,#9601,#9602,#9603,#9604,#9605,#9606,
#9607,#9608,#9609,#9610,#9611,#9612,#9613,#9614,#9615,#9616,#9617,#9618,
#9619,#9620,#9621),#15164);
#15403=SHAPE_REPRESENTATION('',(#8765),#15165);
#15404=SHAPE_REPRESENTATION('',(#8808),#15166);
#15405=SHAPE_REPRESENTATION('',(#8827),#15167);
#15406=SHAPE_REPRESENTATION('',(#8834),#15168);
#15407=SHAPE_REPRESENTATION('',(#8841),#15169);
#15408=SHAPE_REPRESENTATION('',(#8916),#15170);
#15409=SHAPE_REPRESENTATION('',(#8941),#15171);
#15410=SHAPE_REPRESENTATION('',(#8966),#15172);
#15411=SHAPE_REPRESENTATION('',(#9007),#15173);
#15412=SHAPE_REPRESENTATION('',(#9014),#15174);
#15413=SHAPE_REPRESENTATION('',(#9029),#15175);
#15414=SHAPE_REPRESENTATION('',(#9044),#15176);
#15415=SHAPE_REPRESENTATION('',(#9058),#15177);
#15416=SHAPE_REPRESENTATION('',(#9108),#15178);
#15417=SHAPE_REPRESENTATION('',(#9129),#15179);
#15418=SHAPE_REPRESENTATION('',(#9140),#15180);
#15419=SHAPE_REPRESENTATION('',(#9164,#9293,#9294,#9295,#9296,#9297),#15181);
#15420=SHAPE_REPRESENTATION('',(#9165),#15182);
#15421=SHAPE_REPRESENTATION('',(#9185),#15183);
#15422=SHAPE_REPRESENTATION('',(#9205),#15184);
#15423=SHAPE_REPRESENTATION('',(#9222),#15185);
#15424=SHAPE_REPRESENTATION('',(#9276),#15186);
#15425=SHAPE_REPRESENTATION('',(#9298,#9348,#9349),#15187);
#15426=SHAPE_REPRESENTATION('',(#9299),#15188);
#15427=SHAPE_REPRESENTATION('',(#9331),#15189);
#15428=SHAPE_REPRESENTATION('',(#9350),#15190);
#15429=SHAPE_REPRESENTATION('',(#9380,#9622,#9623,#9624,#9625,#9626,#9627,
#9628,#9629,#9630,#9631,#9632),#15191);
#15430=SHAPE_REPRESENTATION('',(#9381),#15192);
#15431=SHAPE_REPRESENTATION('',(#9418),#15193);
#15432=SHAPE_REPRESENTATION('',(#9427),#15194);
#15433=SHAPE_REPRESENTATION('',(#9442),#15195);
#15434=SHAPE_REPRESENTATION('',(#9464),#15196);
#15435=SHAPE_REPRESENTATION('',(#9473),#15197);
#15436=SHAPE_REPRESENTATION('',(#9482),#15198);
#15437=SHAPE_REPRESENTATION('',(#9491),#15199);
#15438=SHAPE_REPRESENTATION('',(#9500),#15200);
#15439=SHAPE_REPRESENTATION('',(#9515),#15201);
#15440=SHAPE_REPRESENTATION('',(#9539),#15202);
#15441=SHAPE_REPRESENTATION('',(#9633,#9669,#9670,#9671),#15203);
#15442=SHAPE_REPRESENTATION('',(#9634),#15204);
#15443=SHAPE_REPRESENTATION('',(#9651),#15205);
#15444=SHAPE_REPRESENTATION('',(#9660),#15206);
#15445=SHAPE_REPRESENTATION('',(#9672,#9746,#9747,#9748,#9749),#15207);
#15446=SHAPE_REPRESENTATION('',(#9673),#15208);
#15447=SHAPE_REPRESENTATION('',(#9713),#15209);
#15448=SHAPE_REPRESENTATION('',(#9723),#15210);
#15449=SHAPE_REPRESENTATION('',(#9729),#15211);
#15450=PRODUCT_DEFINITION_CONTEXT('part definition',#15599,'design');
#15451=PRODUCT_DEFINITION(
'PAT-075','PAT-075',
#15500,#15450);
#15452=PRODUCT_DEFINITION('Base and guide','Base and guide',#15501,#15450);
#15453=PRODUCT_DEFINITION('Base','Base',#15502,#15450);
#15454=PRODUCT_DEFINITION('Fixture mounting plate',
'Fixture mounting plate',#15503,#15450);
#15455=PRODUCT_DEFINITION('Fixture foot strip','Fixture foot strip',#15504,
#15450);
#15456=PRODUCT_DEFINITION('Fixture foot strip (1)',
'Fixture foot strip (1)',#15505,#15450);
#15457=PRODUCT_DEFINITION('Bearing frame','Bearing frame',#15506,#15450);
#15458=PRODUCT_DEFINITION('Front bearing cap','Front bearing cap',#15507,
#15450);
#15459=PRODUCT_DEFINITION('Rear bearing cap','Rear bearing cap',#15508,
#15450);
#15460=PRODUCT_DEFINITION('Linear bearing cap','Linear bearing cap',#15509,
#15450);
#15461=PRODUCT_DEFINITION('Bar specimen envelope',
'Bar specimen envelope',#15510,#15450);
#15462=PRODUCT_DEFINITION('Left bar guide','Left bar guide',#15511,#15450);
#15463=PRODUCT_DEFINITION('Right bar guide','Right bar guide',#15512,#15450);
#15464=PRODUCT_DEFINITION('Closed lever stop','Closed lever stop',#15513,
#15450);
#15465=PRODUCT_DEFINITION('Slotted Extrusion - 20 x 20 x 200 mm',
'Slotted Extrusion - 20 x 20 x 200 mm',#15514,#15450);
#15466=PRODUCT_DEFINITION('Captive slot nut','Captive slot nut',#15515,
#15450);
#15467=PRODUCT_DEFINITION('Flat Washer - M5','Flat Washer - M5',#15516,
#15450);
#15468=PRODUCT_DEFINITION('M5x14 Cap Screw','M5x14 Cap Screw',#15517,#15450);
#15469=PRODUCT_DEFINITION('Sealed Ball Bearing - 10 x 30 x 9 mm',
'Sealed Ball Bearing - 10 x 30 x 9 mm',#15518,#15450);
#15470=PRODUCT_DEFINITION('Inner ring','Inner ring',#15519,#15450);
#15471=PRODUCT_DEFINITION('Outer ring','Outer ring',#15520,#15450);
#15472=PRODUCT_DEFINITION('Balls','Balls',#15521,#15450);
#15473=PRODUCT_DEFINITION('Cage','Cage',#15522,#15450);
#15474=PRODUCT_DEFINITION('Seals 2RS','Seals 2RS',#15523,#15450);
#15475=PRODUCT_DEFINITION('Linear Ball Bushing - 12 x 21 x 30 mm',
'Linear Ball Bushing - 12 x 21 x 30 mm',#15524,#15450);
#15476=PRODUCT_DEFINITION('Steel sleeve','Steel sleeve',#15525,#15450);
#15477=PRODUCT_DEFINITION('Ball retainer (plastic)',
'Ball retainer (plastic)',#15526,#15450);
#15478=PRODUCT_DEFINITION('M4x30 stop screw','M4x30 stop screw',#15527,
#15450);
#15479=PRODUCT_DEFINITION('Operating lever','Operating lever',#15528,#15450);
#15480=PRODUCT_DEFINITION('Lever and spindle','Lever and spindle',#15529,
#15450);
#15481=PRODUCT_DEFINITION('Inner race spacer','Inner race spacer',#15530,
#15450);
#15482=PRODUCT_DEFINITION('Shaft collar','Shaft collar',#15531,#15450);
#15483=PRODUCT_DEFINITION('Lever link pin','Lever link pin',#15532,#15450);
#15484=PRODUCT_DEFINITION('Rear pin spacer','Rear pin spacer',#15533,#15450);
#15485=PRODUCT_DEFINITION('Front pin spacer','Front pin spacer',#15534,
#15450);
#15486=PRODUCT_DEFINITION('Front pin keeper','Front pin keeper',#15535,
#15450);
#15487=PRODUCT_DEFINITION('Rear pin keeper','Rear pin keeper',#15536,#15450);
#15488=PRODUCT_DEFINITION('M4x4 collar screw','M4x4 collar screw',#15537,
#15450);
#15489=PRODUCT_DEFINITION('M4x10 Cap Screw','M4x10 Cap Screw',#15538,#15450);
#15490=PRODUCT_DEFINITION('Cap Screw - M4x16','Cap Screw - M4x16',#15539,
#15450);
#15491=PRODUCT_DEFINITION('Connecting link (1)','Connecting link (1)',#15540,
#15450);
#15492=PRODUCT_DEFINITION('Connecting link','Connecting link',#15541,
#15450);
#15493=PRODUCT_DEFINITION('Link bush','Link bush',#15542,#15450);
#15494=PRODUCT_DEFINITION('Link bush (1)','Link bush (1)',#15543,#15450);
#15495=PRODUCT_DEFINITION('Pressure plunger','Pressure plunger',#15544,
#15450);
#15496=PRODUCT_DEFINITION('Plunger and fork','Plunger and fork',#15545,
#15450);
#15497=PRODUCT_DEFINITION('Fork pin','Fork pin',#15546,#15450);
#15498=PRODUCT_DEFINITION('Elastomer pressure pad installed',
'Elastomer pressure pad installed',#15547,#15450);
#15499=PRODUCT_DEFINITION('Socket Set Screw - M4x6',
'Socket Set Screw - M4x6',#15548,#15450);
#15500=PRODUCT_DEFINITION_FORMATION('',$,#15601);
#15501=PRODUCT_DEFINITION_FORMATION('',$,#15602);
#15502=PRODUCT_DEFINITION_FORMATION('',$,#15603);
#15503=PRODUCT_DEFINITION_FORMATION('',$,#15604);
#15504=PRODUCT_DEFINITION_FORMATION('',$,#15605);
#15505=PRODUCT_DEFINITION_FORMATION('',$,#15606);
#15506=PRODUCT_DEFINITION_FORMATION('',$,#15607);
#15507=PRODUCT_DEFINITION_FORMATION('',$,#15608);
#15508=PRODUCT_DEFINITION_FORMATION('',$,#15609);
#15509=PRODUCT_DEFINITION_FORMATION('',$,#15610);
#15510=PRODUCT_DEFINITION_FORMATION('',$,#15611);
#15511=PRODUCT_DEFINITION_FORMATION('',$,#15612);
#15512=PRODUCT_DEFINITION_FORMATION('',$,#15613);
#15513=PRODUCT_DEFINITION_FORMATION('',$,#15614);
#15514=PRODUCT_DEFINITION_FORMATION('',$,#15615);
#15515=PRODUCT_DEFINITION_FORMATION('',$,#15616);
#15516=PRODUCT_DEFINITION_FORMATION('',$,#15617);
#15517=PRODUCT_DEFINITION_FORMATION('',$,#15618);
#15518=PRODUCT_DEFINITION_FORMATION('',$,#15619);
#15519=PRODUCT_DEFINITION_FORMATION('',$,#15620);
#15520=PRODUCT_DEFINITION_FORMATION('',$,#15621);
#15521=PRODUCT_DEFINITION_FORMATION('',$,#15622);
#15522=PRODUCT_DEFINITION_FORMATION('',$,#15623);
#15523=PRODUCT_DEFINITION_FORMATION('',$,#15624);
#15524=PRODUCT_DEFINITION_FORMATION('',$,#15625);
#15525=PRODUCT_DEFINITION_FORMATION('',$,#15626);
#15526=PRODUCT_DEFINITION_FORMATION('',$,#15627);
#15527=PRODUCT_DEFINITION_FORMATION('',$,#15628);
#15528=PRODUCT_DEFINITION_FORMATION('',$,#15629);
#15529=PRODUCT_DEFINITION_FORMATION('',$,#15630);
#15530=PRODUCT_DEFINITION_FORMATION('',$,#15631);
#15531=PRODUCT_DEFINITION_FORMATION('',$,#15632);
#15532=PRODUCT_DEFINITION_FORMATION('',$,#15633);
#15533=PRODUCT_DEFINITION_FORMATION('',$,#15634);
#15534=PRODUCT_DEFINITION_FORMATION('',$,#15635);
#15535=PRODUCT_DEFINITION_FORMATION('',$,#15636);
#15536=PRODUCT_DEFINITION_FORMATION('',$,#15637);
#15537=PRODUCT_DEFINITION_FORMATION('',$,#15638);
#15538=PRODUCT_DEFINITION_FORMATION('',$,#15639);
#15539=PRODUCT_DEFINITION_FORMATION('',$,#15640);
#15540=PRODUCT_DEFINITION_FORMATION('',$,#15641);
#15541=PRODUCT_DEFINITION_FORMATION('',$,#15642);
#15542=PRODUCT_DEFINITION_FORMATION('',$,#15643);
#15543=PRODUCT_DEFINITION_FORMATION('',$,#15644);
#15544=PRODUCT_DEFINITION_FORMATION('',$,#15645);
#15545=PRODUCT_DEFINITION_FORMATION('',$,#15646);
#15546=PRODUCT_DEFINITION_FORMATION('',$,#15647);
#15547=PRODUCT_DEFINITION_FORMATION('',$,#15648);
#15548=PRODUCT_DEFINITION_FORMATION('',$,#15649);
#15549=PRODUCT_RELATED_PRODUCT_CATEGORY('PAT-075','PAT-075',(#15601));
#15550=PRODUCT_RELATED_PRODUCT_CATEGORY('Base and guide',
'Base and guide',(#15602));
#15551=PRODUCT_RELATED_PRODUCT_CATEGORY('Base','Base',(#15603));
#15552=PRODUCT_RELATED_PRODUCT_CATEGORY('Fixture mounting plate',
'Fixture mounting plate',(#15604));
#15553=PRODUCT_RELATED_PRODUCT_CATEGORY('Fixture foot strip',
'Fixture foot strip',(#15605));
#15554=PRODUCT_RELATED_PRODUCT_CATEGORY('Fixture foot strip (1)',
'Fixture foot strip (1)',(#15606));
#15555=PRODUCT_RELATED_PRODUCT_CATEGORY('Bearing frame','Bearing frame',
(#15607));
#15556=PRODUCT_RELATED_PRODUCT_CATEGORY('Front bearing cap',
'Front bearing cap',(#15608));
#15557=PRODUCT_RELATED_PRODUCT_CATEGORY('Rear bearing cap',
'Rear bearing cap',(#15609));
#15558=PRODUCT_RELATED_PRODUCT_CATEGORY('Linear bearing cap',
'Linear bearing cap',(#15610));
#15559=PRODUCT_RELATED_PRODUCT_CATEGORY('Bar specimen envelope',
'Bar specimen envelope',(#15611));
#15560=PRODUCT_RELATED_PRODUCT_CATEGORY('Left bar guide',
'Left bar guide',(#15612));
#15561=PRODUCT_RELATED_PRODUCT_CATEGORY('Right bar guide',
'Right bar guide',(#15613));
#15562=PRODUCT_RELATED_PRODUCT_CATEGORY('Closed lever stop',
'Closed lever stop',(#15614));
#15563=PRODUCT_RELATED_PRODUCT_CATEGORY(
'Slotted Extrusion - 20 x 20 x 200 mm',
'Slotted Extrusion - 20 x 20 x 200 mm',(#15615));
#15564=PRODUCT_RELATED_PRODUCT_CATEGORY('Captive slot nut',
'Captive slot nut',(#15616));
#15565=PRODUCT_RELATED_PRODUCT_CATEGORY('Flat Washer - M5',
'Flat Washer - M5',(#15617));
#15566=PRODUCT_RELATED_PRODUCT_CATEGORY('M5x14 Cap Screw',
'M5x14 Cap Screw',(#15618));
#15567=PRODUCT_RELATED_PRODUCT_CATEGORY(
'Sealed Ball Bearing - 10 x 30 x 9 mm',
'Sealed Ball Bearing - 10 x 30 x 9 mm',(#15619));
#15568=PRODUCT_RELATED_PRODUCT_CATEGORY('Inner ring','Inner ring',(#15620));
#15569=PRODUCT_RELATED_PRODUCT_CATEGORY('Outer ring','Outer ring',(#15621));
#15570=PRODUCT_RELATED_PRODUCT_CATEGORY('Balls','Balls',(#15622));
#15571=PRODUCT_RELATED_PRODUCT_CATEGORY('Cage','Cage',(#15623));
#15572=PRODUCT_RELATED_PRODUCT_CATEGORY('Seals 2RS','Seals 2RS',(#15624));
#15573=PRODUCT_RELATED_PRODUCT_CATEGORY(
'Linear Ball Bushing - 12 x 21 x 30 mm',
'Linear Ball Bushing - 12 x 21 x 30 mm',(#15625));
#15574=PRODUCT_RELATED_PRODUCT_CATEGORY('Steel sleeve','Steel sleeve',(#15626));
#15575=PRODUCT_RELATED_PRODUCT_CATEGORY('Ball retainer (plastic)',
'Ball retainer (plastic)',(#15627));
#15576=PRODUCT_RELATED_PRODUCT_CATEGORY('M4x30 stop screw',
'M4x30 stop screw',(#15628));
#15577=PRODUCT_RELATED_PRODUCT_CATEGORY('Operating lever',
'Operating lever',(#15629));
#15578=PRODUCT_RELATED_PRODUCT_CATEGORY('Lever and spindle',
'Lever and spindle',(#15630));
#15579=PRODUCT_RELATED_PRODUCT_CATEGORY('Inner race spacer',
'Inner race spacer',(#15631));
#15580=PRODUCT_RELATED_PRODUCT_CATEGORY('Shaft collar','Shaft collar',(#15632));
#15581=PRODUCT_RELATED_PRODUCT_CATEGORY('Lever link pin',
'Lever link pin',(#15633));
#15582=PRODUCT_RELATED_PRODUCT_CATEGORY('Rear pin spacer',
'Rear pin spacer',(#15634));
#15583=PRODUCT_RELATED_PRODUCT_CATEGORY('Front pin spacer',
'Front pin spacer',(#15635));
#15584=PRODUCT_RELATED_PRODUCT_CATEGORY('Front pin keeper',
'Front pin keeper',(#15636));
#15585=PRODUCT_RELATED_PRODUCT_CATEGORY('Rear pin keeper',
'Rear pin keeper',(#15637));
#15586=PRODUCT_RELATED_PRODUCT_CATEGORY('M4x4 collar screw',
'M4x4 collar screw',(#15638));
#15587=PRODUCT_RELATED_PRODUCT_CATEGORY('M4x10 Cap Screw',
'M4x10 Cap Screw',(#15639));
#15588=PRODUCT_RELATED_PRODUCT_CATEGORY('Cap Screw - M4x16',
'Cap Screw - M4x16',(#15640));
#15589=PRODUCT_RELATED_PRODUCT_CATEGORY('Connecting link (1)',
'Connecting link (1)',(#15641));
#15590=PRODUCT_RELATED_PRODUCT_CATEGORY('Connecting link',
'Connecting link',(#15642));
#15591=PRODUCT_RELATED_PRODUCT_CATEGORY('Link bush','Link bush',(#15643));
#15592=PRODUCT_RELATED_PRODUCT_CATEGORY('Link bush (1)','Link bush (1)',
(#15644));
#15593=PRODUCT_RELATED_PRODUCT_CATEGORY('Pressure plunger',
'Pressure plunger',(#15645));
#15594=PRODUCT_RELATED_PRODUCT_CATEGORY('Plunger and fork',
'Plunger and fork',(#15646));
#15595=PRODUCT_RELATED_PRODUCT_CATEGORY('Fork pin','Fork pin',(#15647));
#15596=PRODUCT_RELATED_PRODUCT_CATEGORY(
'Elastomer pressure pad installed','Elastomer pressure pad installed',(#15648));
#15597=PRODUCT_RELATED_PRODUCT_CATEGORY('Socket Set Screw - M4x6',
'Socket Set Screw - M4x6',(#15649));
#15598=APPLICATION_PROTOCOL_DEFINITION('international standard',
'automotive_design',2009,#15599);
#15599=APPLICATION_CONTEXT(
'Core Data for Automotive Mechanical Design Process');
#15600=PRODUCT_CONTEXT('part definition',#15599,'mechanical');
#15601=PRODUCT(
'PAT-075','PAT-075',
'PAT-075',(#15600));
#15602=PRODUCT('Base and guide','Base and guide','Base and guide',(#15600));
#15603=PRODUCT('Base','Base','Base',(#15600));
#15604=PRODUCT('Fixture mounting plate','Fixture mounting plate',
'Fixture mounting plate',(#15600));
#15605=PRODUCT('Fixture foot strip','Fixture foot strip',
'Fixture foot strip',(#15600));
#15606=PRODUCT('Fixture foot strip (1)','Fixture foot strip (1)',
'Fixture foot strip (1)',(#15600));
#15607=PRODUCT('Bearing frame','Bearing frame','Bearing frame',(#15600));
#15608=PRODUCT('Front bearing cap','Front bearing cap',
'Front bearing cap',(#15600));
#15609=PRODUCT('Rear bearing cap','Rear bearing cap','Rear bearing cap',
(#15600));
#15610=PRODUCT('Linear bearing cap','Linear bearing cap',
'Linear bearing cap',(#15600));
#15611=PRODUCT('Bar specimen envelope','Bar specimen envelope',
'Bar specimen envelope',(#15600));
#15612=PRODUCT('Left bar guide','Left bar guide','Left bar guide',(#15600));
#15613=PRODUCT('Right bar guide','Right bar guide','Right bar guide',(#15600));
#15614=PRODUCT('Closed lever stop','Closed lever stop',
'Closed lever stop',(#15600));
#15615=PRODUCT('Slotted Extrusion - 20 x 20 x 200 mm',
'Slotted Extrusion - 20 x 20 x 200 mm',
'Slotted Extrusion - 20 x 20 x 200 mm',(#15600));
#15616=PRODUCT('Captive slot nut','Captive slot nut','Captive slot nut',
(#15600));
#15617=PRODUCT('Flat Washer - M5','Flat Washer - M5','Flat Washer - M5',
(#15600));
#15618=PRODUCT('M5x14 Cap Screw','M5x14 Cap Screw','M5x14 Cap Screw',(#15600));
#15619=PRODUCT('Sealed Ball Bearing - 10 x 30 x 9 mm',
'Sealed Ball Bearing - 10 x 30 x 9 mm',
'Sealed Ball Bearing - 10 x 30 x 9 mm',(#15600));
#15620=PRODUCT('Inner ring','Inner ring','Inner ring',(#15600));
#15621=PRODUCT('Outer ring','Outer ring','Outer ring',(#15600));
#15622=PRODUCT('Balls','Balls','Balls',(#15600));
#15623=PRODUCT('Cage','Cage','Cage',(#15600));
#15624=PRODUCT('Seals 2RS','Seals 2RS','Seals 2RS',(#15600));
#15625=PRODUCT('Linear Ball Bushing - 12 x 21 x 30 mm',
'Linear Ball Bushing - 12 x 21 x 30 mm',
'Linear Ball Bushing - 12 x 21 x 30 mm',(#15600));
#15626=PRODUCT('Steel sleeve','Steel sleeve','Steel sleeve',(#15600));
#15627=PRODUCT('Ball retainer (plastic)','Ball retainer (plastic)',
'Ball retainer (plastic)',(#15600));
#15628=PRODUCT('M4x30 stop screw','M4x30 stop screw','M4x30 stop screw',
(#15600));
#15629=PRODUCT('Operating lever','Operating lever','Operating lever',(#15600));
#15630=PRODUCT('Lever and spindle','Lever and spindle',
'Lever and spindle',(#15600));
#15631=PRODUCT('Inner race spacer','Inner race spacer',
'Inner race spacer',(#15600));
#15632=PRODUCT('Shaft collar','Shaft collar','Shaft collar',(#15600));
#15633=PRODUCT('Lever link pin','Lever link pin','Lever link pin',(#15600));
#15634=PRODUCT('Rear pin spacer','Rear pin spacer','Rear pin spacer',(#15600));
#15635=PRODUCT('Front pin spacer','Front pin spacer','Front pin spacer',
(#15600));
#15636=PRODUCT('Front pin keeper','Front pin keeper','Front pin keeper',
(#15600));
#15637=PRODUCT('Rear pin keeper','Rear pin keeper','Rear pin keeper',(#15600));
#15638=PRODUCT('M4x4 collar screw','M4x4 collar screw',
'M4x4 collar screw',(#15600));
#15639=PRODUCT('M4x10 Cap Screw','M4x10 Cap Screw','M4x10 Cap Screw',(#15600));
#15640=PRODUCT('Cap Screw - M4x16','Cap Screw - M4x16',
'Cap Screw - M4x16',(#15600));
#15641=PRODUCT('Connecting link (1)','Connecting link (1)',
'Connecting link (1)',(#15600));
#15642=PRODUCT('Connecting link','Connecting link','Connecting link',
(#15600));
#15643=PRODUCT('Link bush','Link bush','Link bush',(#15600));
#15644=PRODUCT('Link bush (1)','Link bush (1)','Link bush (1)',(#15600));
#15645=PRODUCT('Pressure plunger','Pressure plunger','Pressure plunger',
(#15600));
#15646=PRODUCT('Plunger and fork','Plunger and fork','Plunger and fork',
(#15600));
#15647=PRODUCT('Fork pin','Fork pin','Fork pin',(#15600));
#15648=PRODUCT('Elastomer pressure pad installed',
'Elastomer pressure pad installed','Elastomer pressure pad installed',(#15600));
#15649=PRODUCT('Socket Set Screw - M4x6','Socket Set Screw - M4x6',
'Socket Set Screw - M4x6',(#15600));
#15650=PRESENTATION_STYLE_ASSIGNMENT((#15656));
#15651=PRESENTATION_STYLE_ASSIGNMENT((#15657));
#15652=PRESENTATION_STYLE_ASSIGNMENT((#15658));
#15653=PRESENTATION_STYLE_ASSIGNMENT((#15659));
#15654=PRESENTATION_STYLE_ASSIGNMENT((#15660));
#15655=PRESENTATION_STYLE_ASSIGNMENT((#15661));
#15656=SURFACE_STYLE_USAGE(.BOTH.,#15662);
#15657=SURFACE_STYLE_USAGE(.BOTH.,#15663);
#15658=SURFACE_STYLE_USAGE(.BOTH.,#15664);
#15659=SURFACE_STYLE_USAGE(.BOTH.,#15665);
#15660=SURFACE_STYLE_USAGE(.BOTH.,#15666);
#15661=SURFACE_STYLE_USAGE(.BOTH.,#15667);
#15662=SURFACE_SIDE_STYLE('',(#15668));
#15663=SURFACE_SIDE_STYLE('',(#15669));
#15664=SURFACE_SIDE_STYLE('',(#15670));
#15665=SURFACE_SIDE_STYLE('',(#15671));
#15666=SURFACE_SIDE_STYLE('',(#15672));
#15667=SURFACE_SIDE_STYLE('',(#15673));
#15668=SURFACE_STYLE_FILL_AREA(#15674);
#15669=SURFACE_STYLE_FILL_AREA(#15675);
#15670=SURFACE_STYLE_FILL_AREA(#15676);
#15671=SURFACE_STYLE_FILL_AREA(#15677);
#15672=SURFACE_STYLE_FILL_AREA(#15678);
#15673=SURFACE_STYLE_FILL_AREA(#15679);
#15674=FILL_AREA_STYLE('Steel - Satin',(#15680));
#15675=FILL_AREA_STYLE('CAD Library Painted - Deep blue',(#15681));
#15676=FILL_AREA_STYLE('CAD Library Painted - Engineering blue',(#15682));
#15677=FILL_AREA_STYLE('CAD Library Painted - Steel gray',(#15683));
#15678=FILL_AREA_STYLE('CAD Library Painted - Light blue',(#15684));
#15679=FILL_AREA_STYLE('CAD Library Painted - Graphite',(#15685));
#15680=FILL_AREA_STYLE_COLOUR('Steel - Satin',#15686);
#15681=FILL_AREA_STYLE_COLOUR('CAD Library Painted - Deep blue',#15687);
#15682=FILL_AREA_STYLE_COLOUR('CAD Library Painted - Engineering blue',
#15688);
#15683=FILL_AREA_STYLE_COLOUR('CAD Library Painted - Steel gray',#15689);
#15684=FILL_AREA_STYLE_COLOUR('CAD Library Painted - Light blue',#15690);
#15685=FILL_AREA_STYLE_COLOUR('CAD Library Painted - Graphite',#15691);
#15686=COLOUR_RGB('Steel - Satin',0.627450980392157,0.627450980392157,0.627450980392157);
#15687=COLOUR_RGB('CAD Library Painted - Deep blue',0.0784313725490196,
0.203921568627451,0.349019607843137);
#15688=COLOUR_RGB('CAD Library Painted - Engineering blue',0.12156862745098,
0.356862745098039,0.6);
#15689=COLOUR_RGB('CAD Library Painted - Steel gray',0.592156862745098,
0.631372549019608,0.67843137254902);
#15690=COLOUR_RGB('CAD Library Painted - Light blue',0.286274509803922,
0.552941176470588,0.780392156862745);
#15691=COLOUR_RGB('CAD Library Painted - Graphite',0.168627450980392,0.192156862745098,
0.231372549019608);
#15692=COLOUR_RGB('Dark Blue',0.08,0.2,0.34);
#15693=FILL_AREA_STYLE_COLOUR('',#15692);
#15694=FILL_AREA_STYLE('',(#15693));
#15695=SURFACE_STYLE_FILL_AREA(#15694);
#15696=SURFACE_SIDE_STYLE('',(#15695));
#15697=SURFACE_STYLE_USAGE(.BOTH.,#15696);
#15698=PRESENTATION_STYLE_ASSIGNMENT((#15697));
#15699=COLOUR_RGB('Light Blue',0.38,0.62,0.78);
#15700=FILL_AREA_STYLE_COLOUR('',#15699);
#15701=FILL_AREA_STYLE('',(#15700));
#15702=SURFACE_STYLE_FILL_AREA(#15701);
#15703=SURFACE_SIDE_STYLE('',(#15702));
#15704=SURFACE_STYLE_USAGE(.BOTH.,#15703);
#15705=PRESENTATION_STYLE_ASSIGNMENT((#15704));
#15706=COLOUR_RGB('Sky Blue',0.24,0.69,0.87);
#15707=FILL_AREA_STYLE_COLOUR('',#15706);
#15708=FILL_AREA_STYLE('',(#15707));
#15709=SURFACE_STYLE_FILL_AREA(#15708);
#15710=SURFACE_SIDE_STYLE('',(#15709));
#15711=SURFACE_STYLE_USAGE(.BOTH.,#15710);
#15712=PRESENTATION_STYLE_ASSIGNMENT((#15711));
#15713=COLOUR_RGB('Grey',0.48,0.52,0.57);
#15714=FILL_AREA_STYLE_COLOUR('',#15713);
#15715=FILL_AREA_STYLE('',(#15714));
#15716=SURFACE_STYLE_FILL_AREA(#15715);
#15717=SURFACE_SIDE_STYLE('',(#15716));
#15718=SURFACE_STYLE_USAGE(.BOTH.,#15717);
#15719=PRESENTATION_STYLE_ASSIGNMENT((#15718));
#15720=COLOUR_RGB('Black',0.12,0.14,0.17);
#15721=FILL_AREA_STYLE_COLOUR('',#15720);
#15722=FILL_AREA_STYLE('',(#15721));
#15723=SURFACE_STYLE_FILL_AREA(#15722);
#15724=SURFACE_SIDE_STYLE('',(#15723));
#15725=SURFACE_STYLE_USAGE(.BOTH.,#15724);
#15726=PRESENTATION_STYLE_ASSIGNMENT((#15725));
#15727=COLOUR_RGB('Off White',0.89,0.88,0.83);
#15728=FILL_AREA_STYLE_COLOUR('',#15727);
#15729=FILL_AREA_STYLE('',(#15728));
#15730=SURFACE_STYLE_FILL_AREA(#15729);
#15731=SURFACE_SIDE_STYLE('',(#15730));
#15732=SURFACE_STYLE_USAGE(.BOTH.,#15731);
#15733=PRESENTATION_STYLE_ASSIGNMENT((#15732));
ENDSEC;
END-ISO-10303-21;
